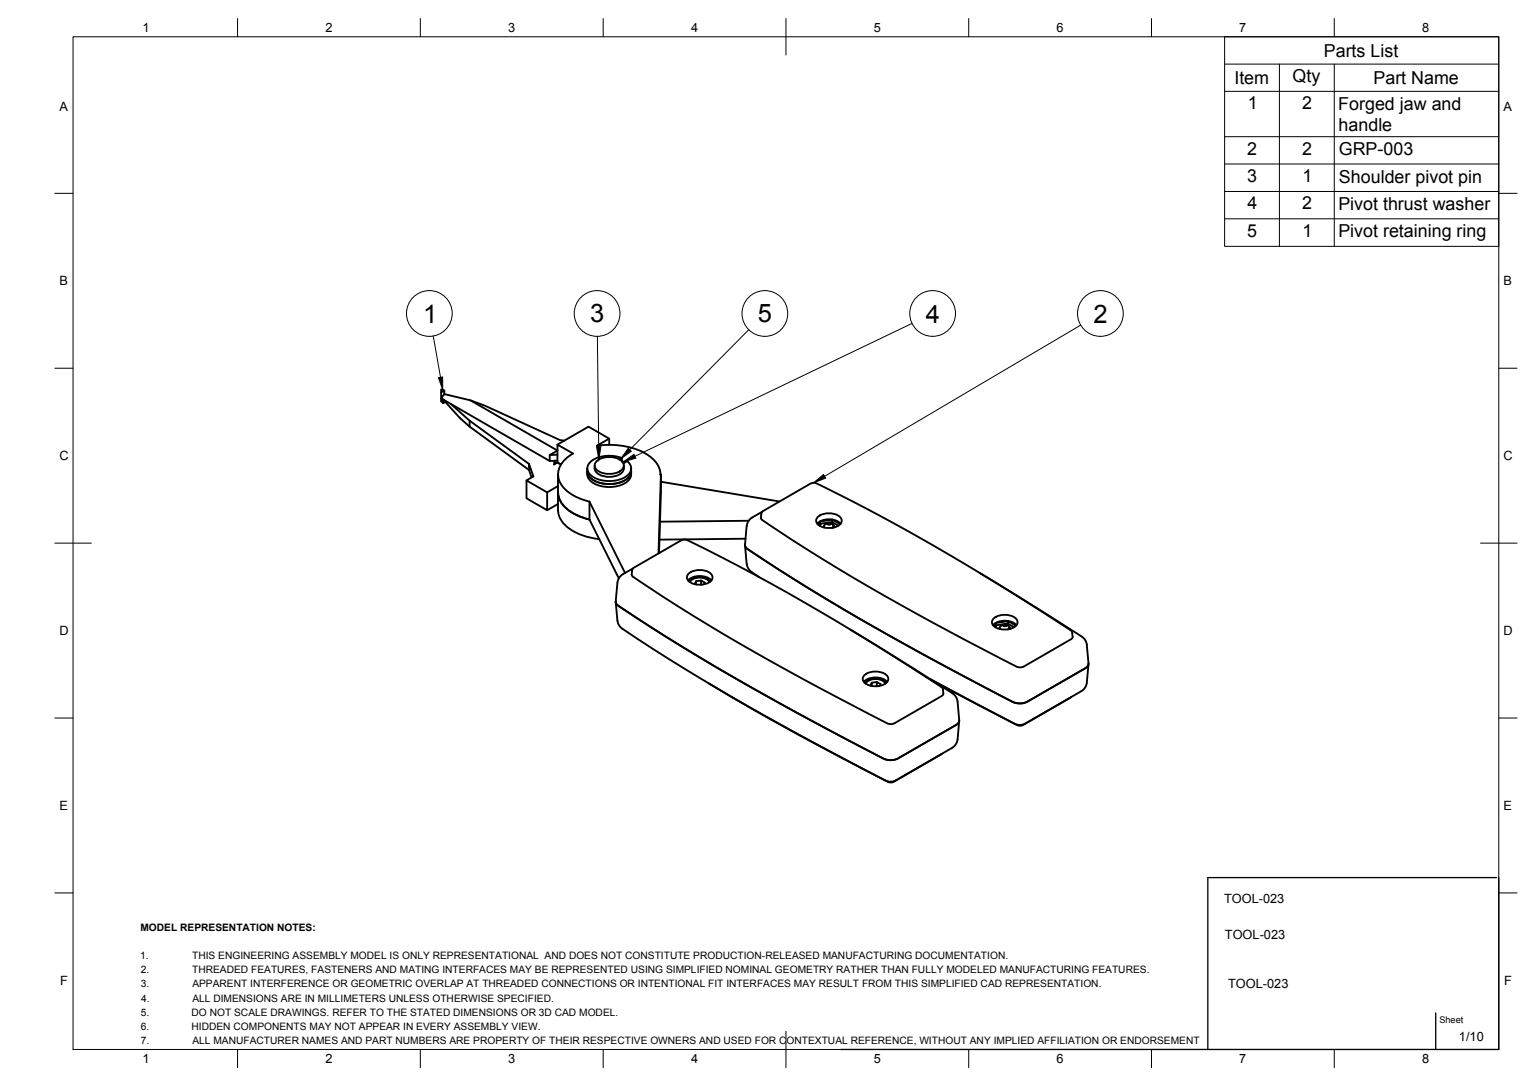
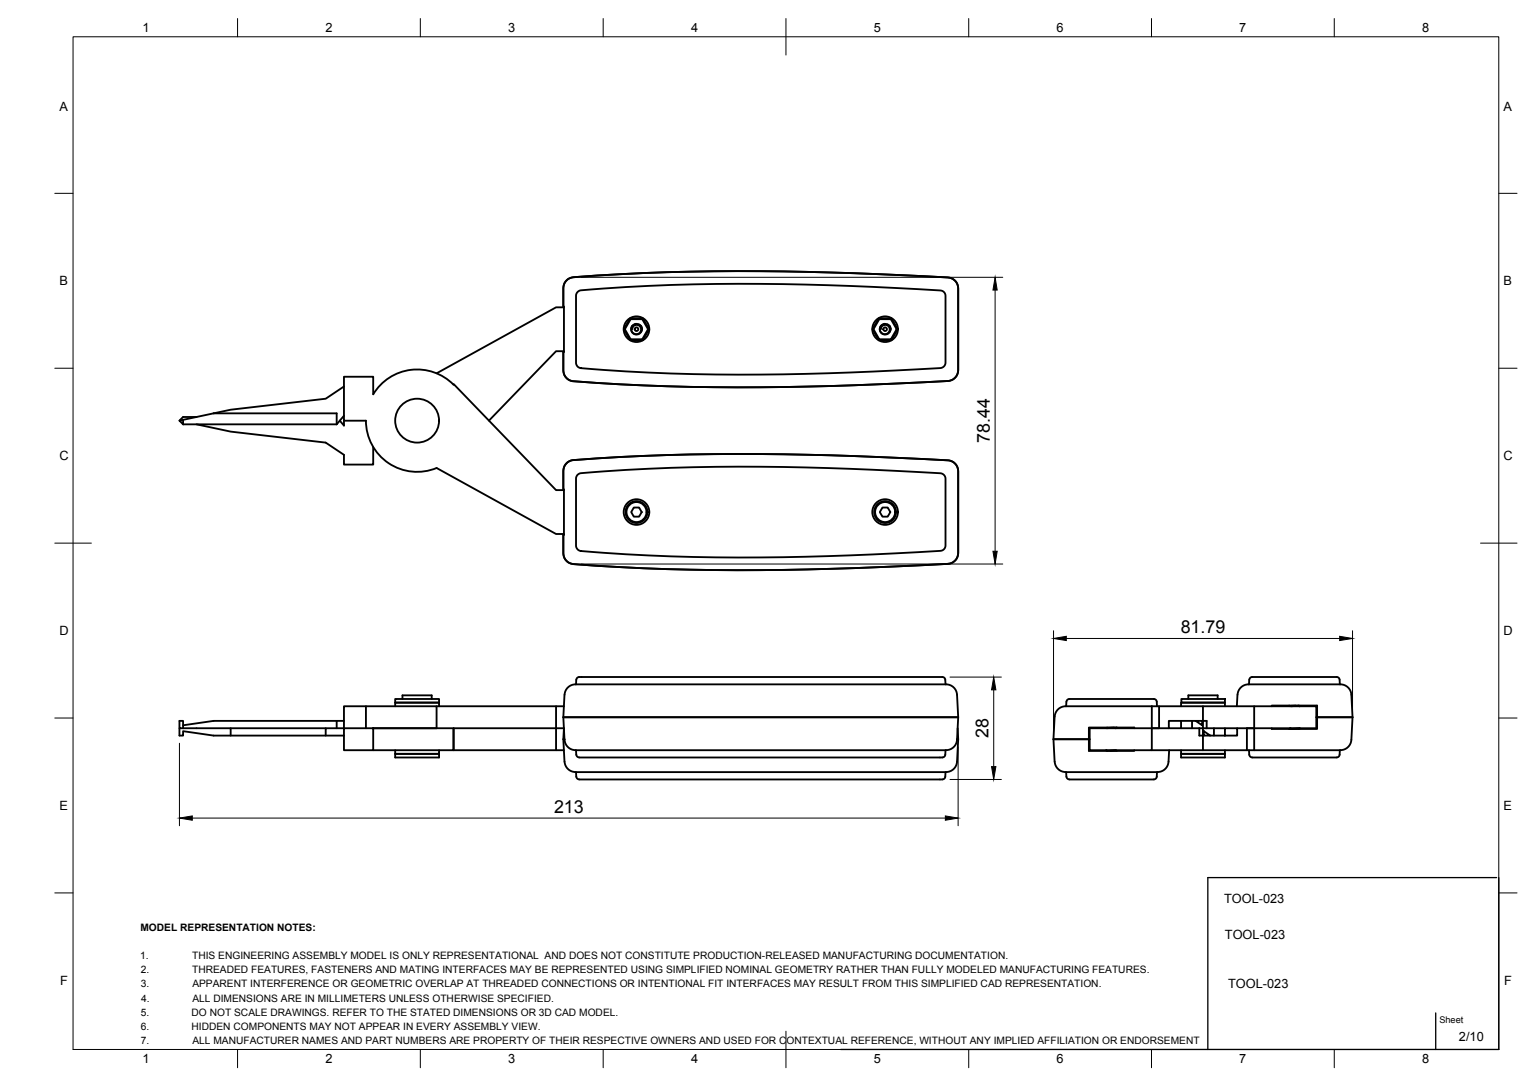
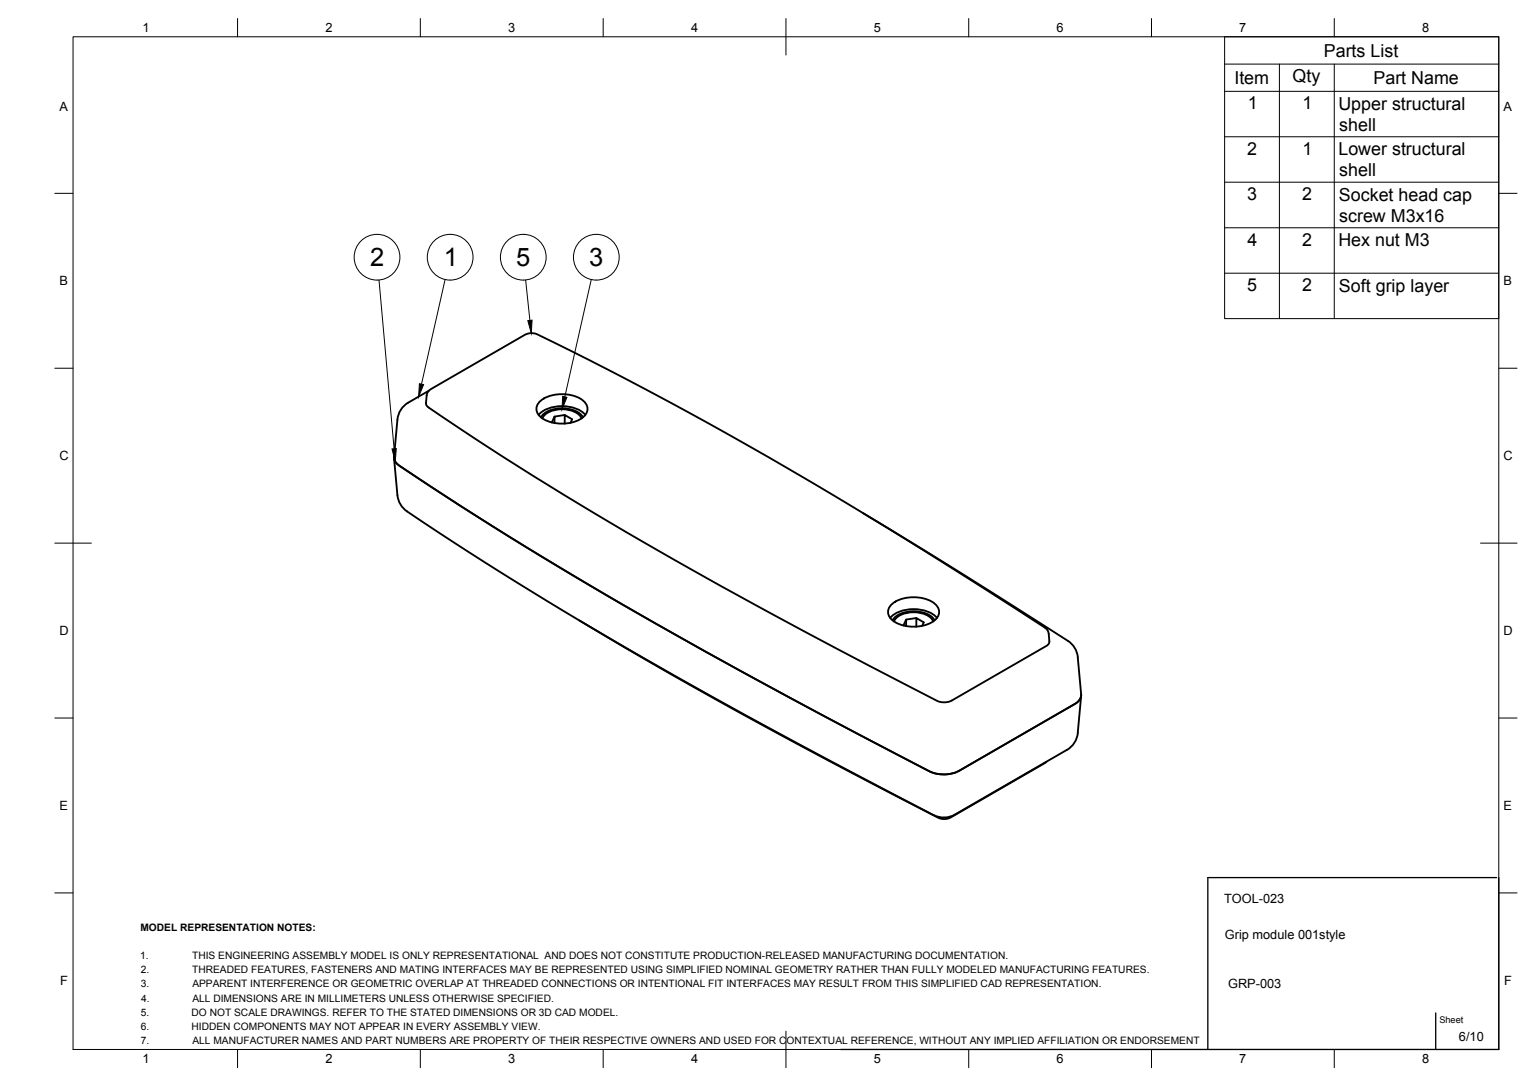
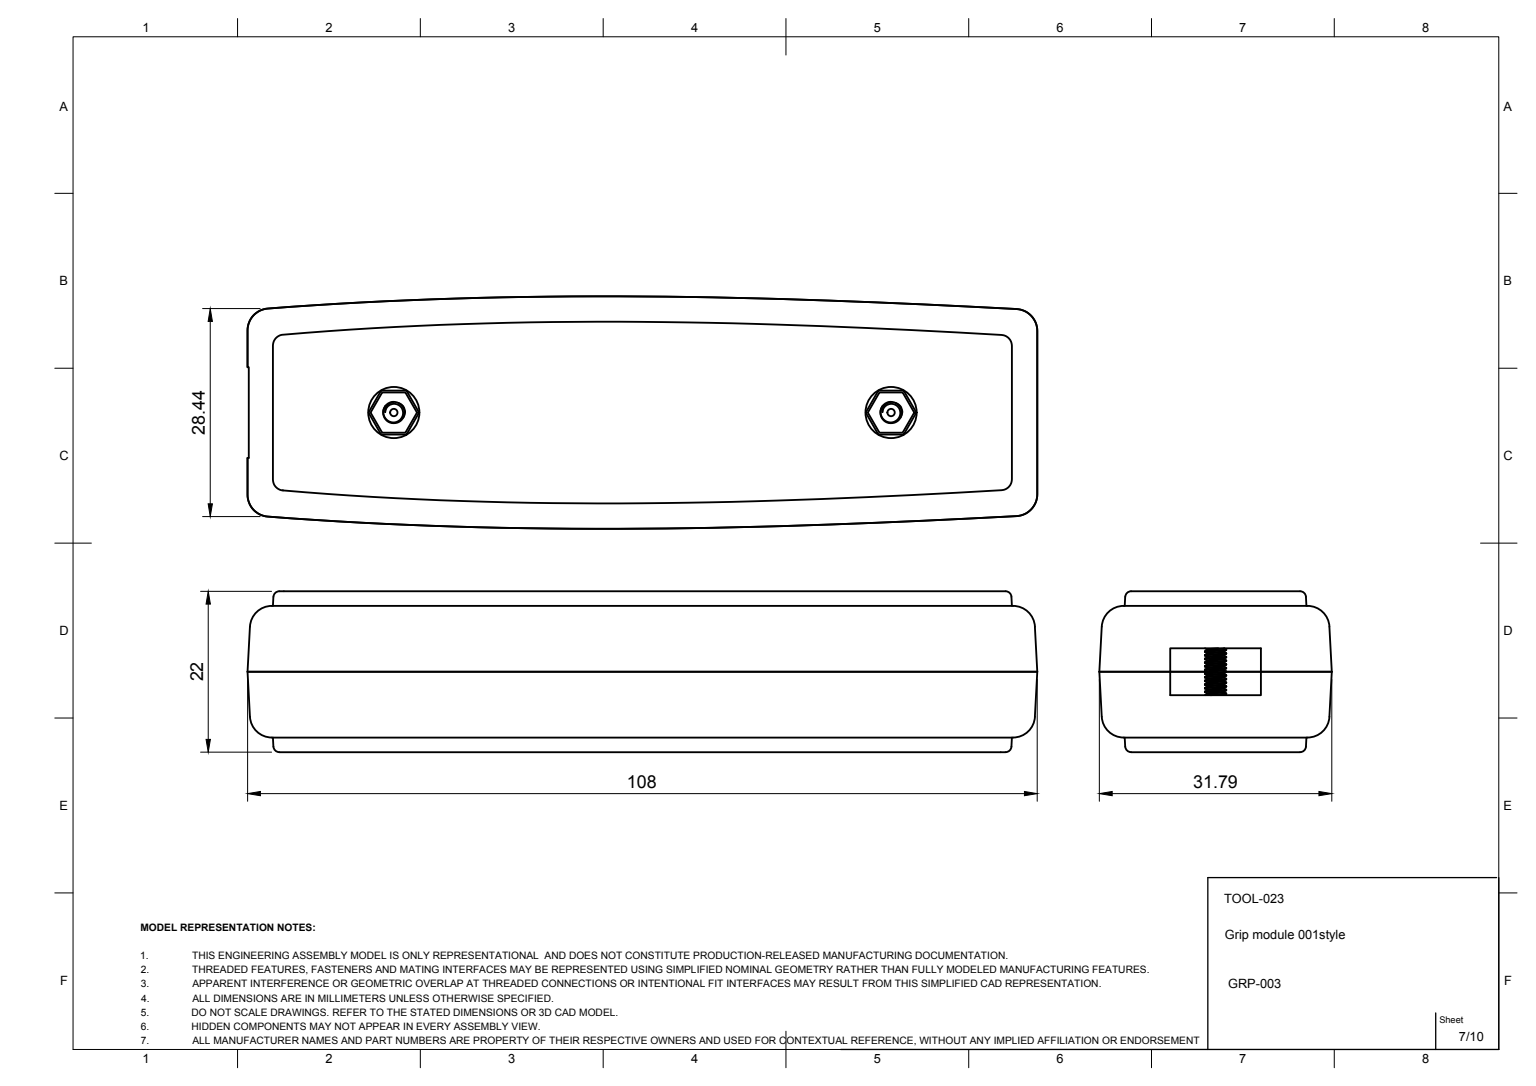
ISO-10303-21;
HEADER;
/* Generated by software containing ST-Developer
 * from STEP Tools, Inc. (www.steptools.com) 
 */

FILE_DESCRIPTION(
/* description */ (''),
/* implementation_level */ '2;1');

FILE_NAME(
/* name */ 'TOOL-023.step',
/* time_stamp */ '2026-11-10T05:40:20-08:00',
/* author */ (''),
/* organization */ (''),
/* preprocessor_version */ 'ST-DEVELOPER v20.2',
/* originating_system */ 'Autodesk Translation Framework v15.17.0.0',
/* authorisation */ '');

FILE_SCHEMA (('AUTOMOTIVE_DESIGN { 1 0 10303 214 3 1 1 }'));
ENDSEC;

DATA;
#10=MECHANICAL_DESIGN_GEOMETRIC_PRESENTATION_REPRESENTATION('',(#572,#573,
#574,#575,#576,#577,#578,#579,#580),#18580);
#11=ITEM_DEFINED_TRANSFORMATION($,$,#6722,#7109);
#12=ITEM_DEFINED_TRANSFORMATION($,$,#6832,#7110);
#13=ITEM_DEFINED_TRANSFORMATION($,$,#6948,#7111);
#14=ITEM_DEFINED_TRANSFORMATION($,$,#7030,#7112);
#15=ITEM_DEFINED_TRANSFORMATION($,$,#7056,#7113);
#16=ITEM_DEFINED_TRANSFORMATION($,$,#6948,#7114);
#17=ITEM_DEFINED_TRANSFORMATION($,$,#7030,#7115);
#18=ITEM_DEFINED_TRANSFORMATION($,$,#7056,#7116);
#19=ITEM_DEFINED_TRANSFORMATION($,$,#6654,#7126);
#20=ITEM_DEFINED_TRANSFORMATION($,$,#6721,#7127);
#21=ITEM_DEFINED_TRANSFORMATION($,$,#6654,#7128);
#22=ITEM_DEFINED_TRANSFORMATION($,$,#6692,#7129);
#23=ITEM_DEFINED_TRANSFORMATION($,$,#7117,#7130);
#24=ITEM_DEFINED_TRANSFORMATION($,$,#6710,#7131);
#25=ITEM_DEFINED_TRANSFORMATION($,$,#6721,#7132);
#26=ITEM_DEFINED_TRANSFORMATION($,$,#7117,#7133);
#27=(
REPRESENTATION_RELATIONSHIP($,$,#18628,#18627)
REPRESENTATION_RELATIONSHIP_WITH_TRANSFORMATION(#11)
SHAPE_REPRESENTATION_RELATIONSHIP()
);
#28=(
REPRESENTATION_RELATIONSHIP($,$,#18629,#18627)
REPRESENTATION_RELATIONSHIP_WITH_TRANSFORMATION(#12)
SHAPE_REPRESENTATION_RELATIONSHIP()
);
#29=(
REPRESENTATION_RELATIONSHIP($,$,#18630,#18627)
REPRESENTATION_RELATIONSHIP_WITH_TRANSFORMATION(#13)
SHAPE_REPRESENTATION_RELATIONSHIP()
);
#30=(
REPRESENTATION_RELATIONSHIP($,$,#18631,#18627)
REPRESENTATION_RELATIONSHIP_WITH_TRANSFORMATION(#14)
SHAPE_REPRESENTATION_RELATIONSHIP()
);
#31=(
REPRESENTATION_RELATIONSHIP($,$,#18632,#18627)
REPRESENTATION_RELATIONSHIP_WITH_TRANSFORMATION(#15)
SHAPE_REPRESENTATION_RELATIONSHIP()
);
#32=(
REPRESENTATION_RELATIONSHIP($,$,#18630,#18627)
REPRESENTATION_RELATIONSHIP_WITH_TRANSFORMATION(#16)
SHAPE_REPRESENTATION_RELATIONSHIP()
);
#33=(
REPRESENTATION_RELATIONSHIP($,$,#18631,#18627)
REPRESENTATION_RELATIONSHIP_WITH_TRANSFORMATION(#17)
SHAPE_REPRESENTATION_RELATIONSHIP()
);
#34=(
REPRESENTATION_RELATIONSHIP($,$,#18632,#18627)
REPRESENTATION_RELATIONSHIP_WITH_TRANSFORMATION(#18)
SHAPE_REPRESENTATION_RELATIONSHIP()
);
#35=(
REPRESENTATION_RELATIONSHIP($,$,#18624,#18623)
REPRESENTATION_RELATIONSHIP_WITH_TRANSFORMATION(#19)
SHAPE_REPRESENTATION_RELATIONSHIP()
);
#36=(
REPRESENTATION_RELATIONSHIP($,$,#18627,#18623)
REPRESENTATION_RELATIONSHIP_WITH_TRANSFORMATION(#20)
SHAPE_REPRESENTATION_RELATIONSHIP()
);
#37=(
REPRESENTATION_RELATIONSHIP($,$,#18624,#18623)
REPRESENTATION_RELATIONSHIP_WITH_TRANSFORMATION(#21)
SHAPE_REPRESENTATION_RELATIONSHIP()
);
#38=(
REPRESENTATION_RELATIONSHIP($,$,#18625,#18623)
REPRESENTATION_RELATIONSHIP_WITH_TRANSFORMATION(#22)
SHAPE_REPRESENTATION_RELATIONSHIP()
);
#39=(
REPRESENTATION_RELATIONSHIP($,$,#18633,#18623)
REPRESENTATION_RELATIONSHIP_WITH_TRANSFORMATION(#23)
SHAPE_REPRESENTATION_RELATIONSHIP()
);
#40=(
REPRESENTATION_RELATIONSHIP($,$,#18626,#18623)
REPRESENTATION_RELATIONSHIP_WITH_TRANSFORMATION(#24)
SHAPE_REPRESENTATION_RELATIONSHIP()
);
#41=(
REPRESENTATION_RELATIONSHIP($,$,#18627,#18623)
REPRESENTATION_RELATIONSHIP_WITH_TRANSFORMATION(#25)
SHAPE_REPRESENTATION_RELATIONSHIP()
);
#42=(
REPRESENTATION_RELATIONSHIP($,$,#18633,#18623)
REPRESENTATION_RELATIONSHIP_WITH_TRANSFORMATION(#26)
SHAPE_REPRESENTATION_RELATIONSHIP()
);
#43=CONTEXT_DEPENDENT_SHAPE_REPRESENTATION(#27,#18606);
#44=CONTEXT_DEPENDENT_SHAPE_REPRESENTATION(#28,#18607);
#45=CONTEXT_DEPENDENT_SHAPE_REPRESENTATION(#29,#18608);
#46=CONTEXT_DEPENDENT_SHAPE_REPRESENTATION(#30,#18609);
#47=CONTEXT_DEPENDENT_SHAPE_REPRESENTATION(#31,#18610);
#48=CONTEXT_DEPENDENT_SHAPE_REPRESENTATION(#32,#18611);
#49=CONTEXT_DEPENDENT_SHAPE_REPRESENTATION(#33,#18612);
#50=CONTEXT_DEPENDENT_SHAPE_REPRESENTATION(#34,#18613);
#51=CONTEXT_DEPENDENT_SHAPE_REPRESENTATION(#35,#18615);
#52=CONTEXT_DEPENDENT_SHAPE_REPRESENTATION(#36,#18616);
#53=CONTEXT_DEPENDENT_SHAPE_REPRESENTATION(#37,#18617);
#54=CONTEXT_DEPENDENT_SHAPE_REPRESENTATION(#38,#18618);
#55=CONTEXT_DEPENDENT_SHAPE_REPRESENTATION(#39,#18619);
#56=CONTEXT_DEPENDENT_SHAPE_REPRESENTATION(#40,#18620);
#57=CONTEXT_DEPENDENT_SHAPE_REPRESENTATION(#41,#18621);
#58=CONTEXT_DEPENDENT_SHAPE_REPRESENTATION(#42,#18622);
#59=NEXT_ASSEMBLY_USAGE_OCCURRENCE('Upper structural shell:1',
'Upper structural shell:1','Upper structural shell:1',#18639,#18640,
'Upper structural shell:1');
#60=NEXT_ASSEMBLY_USAGE_OCCURRENCE('Lower structural shell:1',
'Lower structural shell:1','Lower structural shell:1',#18639,#18641,
'Lower structural shell:1');
#61=NEXT_ASSEMBLY_USAGE_OCCURRENCE('Socket head cap screw M3x16:1',
'Socket head cap screw M3x16:1','Socket head cap screw M3x16:1',#18639,
#18642,'Socket head cap screw M3x16:1');
#62=NEXT_ASSEMBLY_USAGE_OCCURRENCE('Hex nut M3:1','Hex nut M3:1',
'Hex nut M3:1',#18639,#18643,'Hex nut M3:1');
#63=NEXT_ASSEMBLY_USAGE_OCCURRENCE('Soft grip layer:1',
'Soft grip layer:1','Soft grip layer:1',#18639,#18644,
'Soft grip layer:1');
#64=NEXT_ASSEMBLY_USAGE_OCCURRENCE('Socket head cap screw M3x16:2',
'Socket head cap screw M3x16:2','Socket head cap screw M3x16:2',#18639,
#18642,'Socket head cap screw M3x16:2');
#65=NEXT_ASSEMBLY_USAGE_OCCURRENCE('Hex nut M3:2','Hex nut M3:2',
'Hex nut M3:2',#18639,#18643,'Hex nut M3:2');
#66=NEXT_ASSEMBLY_USAGE_OCCURRENCE('Soft grip layer:2',
'Soft grip layer:2','Soft grip layer:2',#18639,#18644,
'Soft grip layer:2');
#67=NEXT_ASSEMBLY_USAGE_OCCURRENCE('Forged jaw and handle:1',
'Forged jaw and handle:1','Forged jaw and handle:1',#18635,#18636,
'Forged jaw and handle:1');
#68=NEXT_ASSEMBLY_USAGE_OCCURRENCE('Grip module:1','Grip module:1',
'Grip module:1',#18635,#18639,'Grip module:1');
#69=NEXT_ASSEMBLY_USAGE_OCCURRENCE('Forged jaw and handle:2',
'Forged jaw and handle:2','Forged jaw and handle:2',#18635,#18636,
'Forged jaw and handle:2');
#70=NEXT_ASSEMBLY_USAGE_OCCURRENCE('Shoulder pivot pin:1',
'Shoulder pivot pin:1','Shoulder pivot pin:1',#18635,#18637,
'Shoulder pivot pin:1');
#71=NEXT_ASSEMBLY_USAGE_OCCURRENCE('Pivot thrust washer:1',
'Pivot thrust washer:1','Pivot thrust washer:1',#18635,#18645,
'Pivot thrust washer:1');
#72=NEXT_ASSEMBLY_USAGE_OCCURRENCE('Pivot retaining ring:1',
'Pivot retaining ring:1','Pivot retaining ring:1',#18635,#18638,
'Pivot retaining ring:1');
#73=NEXT_ASSEMBLY_USAGE_OCCURRENCE('Grip module:2','Grip module:2',
'Grip module:2',#18635,#18639,'Grip module:2');
#74=NEXT_ASSEMBLY_USAGE_OCCURRENCE('Pivot thrust washer:2',
'Pivot thrust washer:2','Pivot thrust washer:2',#18635,#18645,
'Pivot thrust washer:2');
#75=CONICAL_SURFACE('',#7011,0.1,0.785398163397448);
#76=SPHERICAL_SURFACE('',#6795,0.1);
#77=SPHERICAL_SURFACE('',#6798,0.0999999999999998);
#78=SPHERICAL_SURFACE('',#6802,0.0999999999999993);
#79=SPHERICAL_SURFACE('',#6806,0.1);
#80=SPHERICAL_SURFACE('',#6811,0.3);
#81=SPHERICAL_SURFACE('',#6815,0.3);
#82=SPHERICAL_SURFACE('',#6819,0.299999999999999);
#83=SPHERICAL_SURFACE('',#6824,0.3);
#84=SPHERICAL_SURFACE('',#6911,0.1);
#85=SPHERICAL_SURFACE('',#6914,0.0999999999999998);
#86=SPHERICAL_SURFACE('',#6918,0.0999999999999993);
#87=SPHERICAL_SURFACE('',#6922,0.1);
#88=SPHERICAL_SURFACE('',#6927,0.3);
#89=SPHERICAL_SURFACE('',#6931,0.3);
#90=SPHERICAL_SURFACE('',#6935,0.299999999999999);
#91=SPHERICAL_SURFACE('',#6940,0.3);
#92=B_SPLINE_SURFACE_WITH_KNOTS('',3,3,((#8816,#8817,#8818,#8819),(#8820,
#8821,#8822,#8823),(#8824,#8825,#8826,#8827),(#8828,#8829,#8830,#8831),
(#8832,#8833,#8834,#8835)),.UNSPECIFIED.,.F.,.F.,.F.,(4,1,4),(4,4),(0.,
0.571428571428571,1.),(1.0454440030657,3.44967454744645),.UNSPECIFIED.);
#93=B_SPLINE_SURFACE_WITH_KNOTS('',3,3,((#8908,#8909,#8910,#8911),(#8912,
#8913,#8914,#8915),(#8916,#8917,#8918,#8919),(#8920,#8921,#8922,#8923),
(#8924,#8925,#8926,#8927)),.UNSPECIFIED.,.F.,.F.,.F.,(4,1,4),(4,4),(0.,
0.571428571428571,1.),(7.24519303641511,9.95046872158573),.UNSPECIFIED.);
#94=B_SPLINE_SURFACE_WITH_KNOTS('',3,3,((#9789,#9790,#9791,#9792),(#9793,
#9794,#9795,#9796),(#9797,#9798,#9799,#9800),(#9801,#9802,#9803,#9804)),
 .UNSPECIFIED.,.F.,.F.,.F.,(4,4),(4,4),(0.0705535719740953,0.323522444336189),
(0.0117434863834119,0.684857763552191),.UNSPECIFIED.);
#95=B_SPLINE_SURFACE_WITH_KNOTS('',3,3,((#9809,#9810,#9811,#9812),(#9813,
#9814,#9815,#9816),(#9817,#9818,#9819,#9820),(#9821,#9822,#9823,#9824)),
 .UNSPECIFIED.,.F.,.F.,.F.,(4,4),(4,4),(0.0262419052680539,0.0545428296147404),
(0.0121538053864343,0.684980602226481),.UNSPECIFIED.);
#96=B_SPLINE_SURFACE_WITH_KNOTS('',3,3,((#9834,#9835,#9836,#9837),(#9838,
#9839,#9840,#9841),(#9842,#9843,#9844,#9845),(#9846,#9847,#9848,#9849),
(#9850,#9851,#9852,#9853)),.UNSPECIFIED.,.F.,.F.,.F.,(4,1,4),(4,4),(0.,
0.571428571428571,1.),(0.752061768057538,3.45733745322815),
 .UNSPECIFIED.);
#97=B_SPLINE_SURFACE_WITH_KNOTS('',3,3,((#9854,#9855,#9856,#9857),(#9858,
#9859,#9860,#9861),(#9862,#9863,#9864,#9865),(#9866,#9867,#9868,#9869),
(#9870,#9871,#9872,#9873)),.UNSPECIFIED.,.F.,.F.,.F.,(4,1,4),(4,4),(0.,
0.571428571428571,1.),(0.283259008618247,0.557056952888827),
 .UNSPECIFIED.);
#98=B_SPLINE_SURFACE_WITH_KNOTS('',3,3,((#9887,#9888,#9889,#9890),(#9891,
#9892,#9893,#9894),(#9895,#9896,#9897,#9898),(#9899,#9900,#9901,#9902)),
 .UNSPECIFIED.,.F.,.F.,.F.,(4,4),(4,4),(0.67647755566375,0.929446428026011),
(0.0117434863436937,0.684857763580381),.UNSPECIFIED.);
#99=B_SPLINE_SURFACE_WITH_KNOTS('',3,3,((#9903,#9904,#9905,#9906),(#9907,
#9908,#9909,#9910),(#9911,#9912,#9913,#9914),(#9915,#9916,#9917,#9918)),
 .UNSPECIFIED.,.F.,.F.,.F.,(4,4),(4,4),(0.945457170385156,0.973758094731946),
(0.0121538053598088,0.684980602226481),.UNSPECIFIED.);
#100=B_SPLINE_SURFACE_WITH_KNOTS('',3,3,((#10002,#10003,#10004,#10005),
(#10006,#10007,#10008,#10009),(#10010,#10011,#10012,#10013),(#10014,#10015,
#10016,#10017)),.UNSPECIFIED.,.F.,.F.,.F.,(4,4),(4,4),(0.341142793678372,
0.658675488550287),(0.0116221239297273,0.684255166525269),.UNSPECIFIED.);
#101=B_SPLINE_SURFACE_WITH_KNOTS('',3,3,((#10022,#10023,#10024,#10025),
(#10026,#10027,#10028,#10029),(#10030,#10031,#10032,#10033),(#10034,#10035,
#10036,#10037),(#10038,#10039,#10040,#10041)),.UNSPECIFIED.,.F.,.F.,.F.,
(4,1,4),(4,4),(0.,0.571428571428571,1.),(3.65450559744172,7.0548588409572),
 .UNSPECIFIED.);
#102=B_SPLINE_SURFACE_WITH_KNOTS('',3,3,((#10051,#10052,#10053,#10054),
(#10055,#10056,#10057,#10058),(#10059,#10060,#10061,#10062),(#10063,#10064,
#10065,#10066),(#10067,#10068,#10069,#10070)),.UNSPECIFIED.,.F.,.F.,.F.,
(4,1,4),(4,4),(0.,0.571428571428571,1.),(3.64767164868607,7.04802489220155),
 .UNSPECIFIED.);
#103=B_SPLINE_SURFACE_WITH_KNOTS('',3,3,((#10075,#10076,#10077,#10078),
(#10079,#10080,#10081,#10082),(#10083,#10084,#10085,#10086),(#10087,#10088,
#10089,#10090)),.UNSPECIFIED.,.F.,.F.,.F.,(4,4),(4,4),(0.341324511449716,
0.658857206321627),(0.0116221214776208,0.684255166525269),.UNSPECIFIED.);
#104=B_SPLINE_SURFACE_WITH_KNOTS('',3,3,((#10135,#10136,#10137,#10138),
(#10139,#10140,#10141,#10142),(#10143,#10144,#10145,#10146),(#10147,#10148,
#10149,#10150)),.UNSPECIFIED.,.F.,.F.,.F.,(4,4),(4,4),(0.676316266718331,
0.901708040522105),(0.0117102006467275,0.68495201331719),.UNSPECIFIED.);
#105=B_SPLINE_SURFACE_WITH_KNOTS('',3,3,((#10155,#10156,#10157,#10158),
(#10159,#10160,#10161,#10162),(#10163,#10164,#10165,#10166),(#10167,#10168,
#10169,#10170),(#10171,#10172,#10173,#10174)),.UNSPECIFIED.,.F.,.F.,.F.,
(4,1,4),(4,4),(0.,0.571428571428571,1.),(7.25285594219682,9.65708648657758),
 .UNSPECIFIED.);
#106=B_SPLINE_SURFACE_WITH_KNOTS('',3,3,((#10184,#10185,#10186,#10187),
(#10188,#10189,#10190,#10191),(#10192,#10193,#10194,#10195),(#10196,#10197,
#10198,#10199)),.UNSPECIFIED.,.F.,.F.,.F.,(4,4),(4,4),(0.0982919594778951,
0.323683733281714),(0.0117102006467272,0.68495201331719),.UNSPECIFIED.);
#107=B_SPLINE_SURFACE_WITH_KNOTS('',3,3,((#10274,#10275,#10276,#10277),
(#10278,#10279,#10280,#10281),(#10282,#10283,#10284,#10285),(#10286,#10287,
#10288,#10289)),.UNSPECIFIED.,.F.,.F.,.F.,(4,4),(4,4),(0.917922863855343,
0.974411608827007),(0.0122403473423911,0.685344304754238),.UNSPECIFIED.);
#108=B_SPLINE_SURFACE_WITH_KNOTS('',3,3,((#10299,#10300,#10301,#10302),
(#10303,#10304,#10305,#10306),(#10307,#10308,#10309,#10310),(#10311,#10312,
#10313,#10314),(#10315,#10316,#10317,#10318)),.UNSPECIFIED.,.F.,.F.,.F.,
(4,1,4),(4,4),(0.,0.571428571428571,1.),(9.85085636625011,10.4271318523291),
 .UNSPECIFIED.);
#109=B_SPLINE_SURFACE_WITH_KNOTS('',3,3,((#10332,#10333,#10334,#10335),
(#10336,#10337,#10338,#10339),(#10340,#10341,#10342,#10343),(#10344,#10345,
#10346,#10347)),.UNSPECIFIED.,.F.,.F.,.F.,(4,4),(4,4),(0.025588391172993,
0.0820771361446569),(0.0122403473423911,0.685344304754238),
 .UNSPECIFIED.);
#110=B_SPLINE_SURFACE_WITH_KNOTS('',3,3,((#10357,#10358,#10359,#10360),
(#10361,#10362,#10363,#10364),(#10365,#10366,#10367,#10368),(#10369,#10370,
#10371,#10372),(#10373,#10374,#10375,#10376)),.UNSPECIFIED.,.F.,.F.,.F.,
(4,1,4),(4,4),(0.,0.571428571428571,1.),(0.27539863731415,0.851674123393175),
 .UNSPECIFIED.);
#111=B_SPLINE_SURFACE_WITH_KNOTS('',3,3,((#10390,#10391,#10392,#10393),
(#10394,#10395,#10396,#10397),(#10398,#10399,#10400,#10401),(#10402,#10403,
#10404,#10405),(#10406,#10407,#10408,#10409)),.UNSPECIFIED.,.F.,.F.,.F.,
(4,1,4),(4,4),(0.,0.571428571428571,1.),(0.00944995813270487,0.618489359031386),
 .UNSPECIFIED.);
#112=B_SPLINE_SURFACE_WITH_KNOTS('',3,3,((#10416,#10417,#10418,#10419),
(#10420,#10421,#10422,#10423),(#10424,#10425,#10426,#10427),(#10428,#10429,
#10430,#10431),(#10432,#10433,#10434,#10435)),.UNSPECIFIED.,.F.,.F.,.F.,
(4,1,4),(4,4),(0.,0.571428571428571,1.),(0.00908570715245136,0.618164468641375),
 .UNSPECIFIED.);
#113=B_SPLINE_SURFACE_WITH_KNOTS('',3,3,((#10440,#10441,#10442,#10443),
(#10444,#10445,#10446,#10447),(#10448,#10449,#10450,#10451),(#10452,#10453,
#10454,#10455),(#10456,#10457,#10458,#10459)),.UNSPECIFIED.,.F.,.F.,.F.,
(4,1,4),(4,4),(0.,0.571428571428571,1.),(0.0091183540525243,0.618164468641375),
 .UNSPECIFIED.);
#114=B_SPLINE_SURFACE_WITH_KNOTS('',3,3,((#10464,#10465,#10466,#10467),
(#10468,#10469,#10470,#10471),(#10472,#10473,#10474,#10475),(#10476,#10477,
#10478,#10479),(#10480,#10481,#10482,#10483)),.UNSPECIFIED.,.F.,.F.,.F.,
(4,1,4),(4,4),(0.,0.571428571428571,1.),(10.1454735367545,10.419271481025),
 .UNSPECIFIED.);
#115=B_SPLINE_SURFACE_WITH_KNOTS('',3,3,((#10484,#10485,#10486,#10487),
(#10488,#10489,#10490,#10491),(#10492,#10493,#10494,#10495),(#10496,#10497,
#10498,#10499),(#10500,#10501,#10502,#10503)),.UNSPECIFIED.,.F.,.F.,.F.,
(4,1,4),(4,4),(0.,0.571428571428571,1.),(0.0094045468285345,0.618489359031386),
 .UNSPECIFIED.);
#116=B_SPLINE_SURFACE_WITH_KNOTS('',3,3,((#10529,#10530,#10531,#10532),
(#10533,#10534,#10535,#10536),(#10537,#10538,#10539,#10540),(#10541,#10542,
#10543,#10544),(#10545,#10546,#10547,#10548)),.UNSPECIFIED.,.F.,.F.,.F.,
(4,1,4),(4,4),(0.,0.571428571428571,1.),(-0.00535061636073277,0.618489359031386),
 .UNSPECIFIED.);
#117=B_SPLINE_SURFACE_WITH_KNOTS('',3,3,((#10567,#10568,#10569,#10570,#10571),
(#10572,#10573,#10574,#10575,#10576),(#10577,#10578,#10579,#10580,#10581),
(#10582,#10583,#10584,#10585,#10586),(#10587,#10588,#10589,#10590,#10591)),
 .UNSPECIFIED.,.F.,.F.,.F.,(4,1,4),(4,1,4),(0.,0.571428571428571,1.),(0.283259008618247,
4.63063308449434,10.4271318523291),.UNSPECIFIED.);
#118=B_SPLINE_SURFACE_WITH_KNOTS('',3,3,((#10602,#10603,#10604,#10605),
(#10606,#10607,#10608,#10609),(#10610,#10611,#10612,#10613),(#10614,#10615,
#10616,#10617),(#10618,#10619,#10620,#10621)),.UNSPECIFIED.,.F.,.F.,.F.,
(4,1,4),(4,4),(0.,0.571428571428571,1.),(-0.00578978989683084,0.618164468641375),
 .UNSPECIFIED.);
#119=B_SPLINE_SURFACE_WITH_KNOTS('',3,3,((#10630,#10631,#10632,#10633),
(#10634,#10635,#10636,#10637),(#10638,#10639,#10640,#10641),(#10642,#10643,
#10644,#10645),(#10646,#10647,#10648,#10649)),.UNSPECIFIED.,.F.,.F.,.F.,
(4,1,4),(4,4),(0.,0.571428571428571,1.),(-0.00569189159989896,0.618164468641375),
 .UNSPECIFIED.);
#120=B_SPLINE_SURFACE_WITH_KNOTS('',3,3,((#10658,#10659,#10660,#10661,#10662),
(#10663,#10664,#10665,#10666,#10667),(#10668,#10669,#10670,#10671,#10672),
(#10673,#10674,#10675,#10676,#10677),(#10678,#10679,#10680,#10681,#10682)),
 .UNSPECIFIED.,.F.,.F.,.F.,(4,1,4),(4,1,4),(0.,0.571428571428571,1.),(0.27539863731415,
4.62277271319024,10.419271481025),.UNSPECIFIED.);
#121=B_SPLINE_SURFACE_WITH_KNOTS('',3,3,((#10693,#10694,#10695,#10696),
(#10697,#10698,#10699,#10700),(#10701,#10702,#10703,#10704),(#10705,#10706,
#10707,#10708),(#10709,#10710,#10711,#10712)),.UNSPECIFIED.,.F.,.F.,.F.,
(4,1,4),(4,4),(0.,0.571428571428571,1.),(-0.0054868135546625,0.618489359031386),
 .UNSPECIFIED.);
#122=B_SPLINE_SURFACE_WITH_KNOTS('',3,3,((#10721,#10722,#10723,#10724),
(#10725,#10726,#10727,#10728),(#10729,#10730,#10731,#10732),(#10733,#10734,
#10735,#10736)),.UNSPECIFIED.,.F.,.F.,.F.,(4,4),(4,4),(0.026239262514127,
0.974414173651419),(0.,0.685344304754238),.UNSPECIFIED.);
#123=B_SPLINE_SURFACE_WITH_KNOTS('',3,3,((#10739,#10740,#10741,#10742),
(#10743,#10744,#10745,#10746),(#10747,#10748,#10749,#10750),(#10751,#10752,
#10753,#10754)),.UNSPECIFIED.,.F.,.F.,.F.,(4,4),(4,4),(0.0255858263485814,
0.973760737485873),(0.,0.685344304754238),.UNSPECIFIED.);
#124=B_SPLINE_SURFACE_WITH_KNOTS('',3,3,((#10861,#10862,#10863,#10864),
(#10865,#10866,#10867,#10868),(#10869,#10870,#10871,#10872),(#10873,#10874,
#10875,#10876),(#10877,#10878,#10879,#10880)),.UNSPECIFIED.,.F.,.F.,.F.,
(4,1,4),(4,4),(0.,0.571428571428571,1.),(1.0454440030657,3.44967454744645),
 .UNSPECIFIED.);
#125=B_SPLINE_SURFACE_WITH_KNOTS('',3,3,((#10953,#10954,#10955,#10956),
(#10957,#10958,#10959,#10960),(#10961,#10962,#10963,#10964),(#10965,#10966,
#10967,#10968),(#10969,#10970,#10971,#10972)),.UNSPECIFIED.,.F.,.F.,.F.,
(4,1,4),(4,4),(0.,0.571428571428571,1.),(7.24519303641511,9.95046872158573),
 .UNSPECIFIED.);
#126=B_SPLINE_SURFACE_WITH_KNOTS('',3,3,((#11894,#11895,#11896,#11897),
(#11898,#11899,#11900,#11901),(#11902,#11903,#11904,#11905),(#11906,#11907,
#11908,#11909)),.UNSPECIFIED.,.F.,.F.,.F.,(4,4),(4,4),(0.0705535719740953,
0.323522444336189),(0.0117434863834119,0.684857763552191),.UNSPECIFIED.);
#127=B_SPLINE_SURFACE_WITH_KNOTS('',3,3,((#11914,#11915,#11916,#11917),
(#11918,#11919,#11920,#11921),(#11922,#11923,#11924,#11925),(#11926,#11927,
#11928,#11929)),.UNSPECIFIED.,.F.,.F.,.F.,(4,4),(4,4),(0.0262419052680539,
0.0545428296147404),(0.0121538053864343,0.684980602226481),
 .UNSPECIFIED.);
#128=B_SPLINE_SURFACE_WITH_KNOTS('',3,3,((#11939,#11940,#11941,#11942),
(#11943,#11944,#11945,#11946),(#11947,#11948,#11949,#11950),(#11951,#11952,
#11953,#11954),(#11955,#11956,#11957,#11958)),.UNSPECIFIED.,.F.,.F.,.F.,
(4,1,4),(4,4),(0.,0.571428571428571,1.),(0.752061768057538,3.45733745322815),
 .UNSPECIFIED.);
#129=B_SPLINE_SURFACE_WITH_KNOTS('',3,3,((#11959,#11960,#11961,#11962),
(#11963,#11964,#11965,#11966),(#11967,#11968,#11969,#11970),(#11971,#11972,
#11973,#11974),(#11975,#11976,#11977,#11978)),.UNSPECIFIED.,.F.,.F.,.F.,
(4,1,4),(4,4),(0.,0.571428571428571,1.),(0.283259008618247,0.557056952888827),
 .UNSPECIFIED.);
#130=B_SPLINE_SURFACE_WITH_KNOTS('',3,3,((#11992,#11993,#11994,#11995),
(#11996,#11997,#11998,#11999),(#12000,#12001,#12002,#12003),(#12004,#12005,
#12006,#12007)),.UNSPECIFIED.,.F.,.F.,.F.,(4,4),(4,4),(0.67647755566375,
0.929446428026011),(0.0117434863436937,0.684857763580381),.UNSPECIFIED.);
#131=B_SPLINE_SURFACE_WITH_KNOTS('',3,3,((#12008,#12009,#12010,#12011),
(#12012,#12013,#12014,#12015),(#12016,#12017,#12018,#12019),(#12020,#12021,
#12022,#12023)),.UNSPECIFIED.,.F.,.F.,.F.,(4,4),(4,4),(0.945457170385156,
0.973758094731946),(0.0121538053598088,0.684980602226481),.UNSPECIFIED.);
#132=B_SPLINE_SURFACE_WITH_KNOTS('',3,3,((#12107,#12108,#12109,#12110),
(#12111,#12112,#12113,#12114),(#12115,#12116,#12117,#12118),(#12119,#12120,
#12121,#12122)),.UNSPECIFIED.,.F.,.F.,.F.,(4,4),(4,4),(0.341142793678372,
0.658675488550287),(0.0116221239297273,0.684255166525269),.UNSPECIFIED.);
#133=B_SPLINE_SURFACE_WITH_KNOTS('',3,3,((#12127,#12128,#12129,#12130),
(#12131,#12132,#12133,#12134),(#12135,#12136,#12137,#12138),(#12139,#12140,
#12141,#12142),(#12143,#12144,#12145,#12146)),.UNSPECIFIED.,.F.,.F.,.F.,
(4,1,4),(4,4),(0.,0.571428571428571,1.),(3.65450559744172,7.0548588409572),
 .UNSPECIFIED.);
#134=B_SPLINE_SURFACE_WITH_KNOTS('',3,3,((#12156,#12157,#12158,#12159),
(#12160,#12161,#12162,#12163),(#12164,#12165,#12166,#12167),(#12168,#12169,
#12170,#12171),(#12172,#12173,#12174,#12175)),.UNSPECIFIED.,.F.,.F.,.F.,
(4,1,4),(4,4),(0.,0.571428571428571,1.),(3.64767164868607,7.04802489220155),
 .UNSPECIFIED.);
#135=B_SPLINE_SURFACE_WITH_KNOTS('',3,3,((#12180,#12181,#12182,#12183),
(#12184,#12185,#12186,#12187),(#12188,#12189,#12190,#12191),(#12192,#12193,
#12194,#12195)),.UNSPECIFIED.,.F.,.F.,.F.,(4,4),(4,4),(0.341324511449716,
0.658857206321627),(0.0116221214776208,0.684255166525269),.UNSPECIFIED.);
#136=B_SPLINE_SURFACE_WITH_KNOTS('',3,3,((#12240,#12241,#12242,#12243),
(#12244,#12245,#12246,#12247),(#12248,#12249,#12250,#12251),(#12252,#12253,
#12254,#12255)),.UNSPECIFIED.,.F.,.F.,.F.,(4,4),(4,4),(0.676316266718331,
0.901708040522105),(0.0117102006467275,0.68495201331719),.UNSPECIFIED.);
#137=B_SPLINE_SURFACE_WITH_KNOTS('',3,3,((#12260,#12261,#12262,#12263),
(#12264,#12265,#12266,#12267),(#12268,#12269,#12270,#12271),(#12272,#12273,
#12274,#12275),(#12276,#12277,#12278,#12279)),.UNSPECIFIED.,.F.,.F.,.F.,
(4,1,4),(4,4),(0.,0.571428571428571,1.),(7.25285594219682,9.65708648657758),
 .UNSPECIFIED.);
#138=B_SPLINE_SURFACE_WITH_KNOTS('',3,3,((#12289,#12290,#12291,#12292),
(#12293,#12294,#12295,#12296),(#12297,#12298,#12299,#12300),(#12301,#12302,
#12303,#12304)),.UNSPECIFIED.,.F.,.F.,.F.,(4,4),(4,4),(0.0982919594778951,
0.323683733281714),(0.0117102006467272,0.68495201331719),.UNSPECIFIED.);
#139=B_SPLINE_SURFACE_WITH_KNOTS('',3,3,((#12379,#12380,#12381,#12382),
(#12383,#12384,#12385,#12386),(#12387,#12388,#12389,#12390),(#12391,#12392,
#12393,#12394)),.UNSPECIFIED.,.F.,.F.,.F.,(4,4),(4,4),(0.917922863855343,
0.974411608827007),(0.0122403473423911,0.685344304754238),.UNSPECIFIED.);
#140=B_SPLINE_SURFACE_WITH_KNOTS('',3,3,((#12404,#12405,#12406,#12407),
(#12408,#12409,#12410,#12411),(#12412,#12413,#12414,#12415),(#12416,#12417,
#12418,#12419),(#12420,#12421,#12422,#12423)),.UNSPECIFIED.,.F.,.F.,.F.,
(4,1,4),(4,4),(0.,0.571428571428571,1.),(9.85085636625011,10.4271318523291),
 .UNSPECIFIED.);
#141=B_SPLINE_SURFACE_WITH_KNOTS('',3,3,((#12437,#12438,#12439,#12440),
(#12441,#12442,#12443,#12444),(#12445,#12446,#12447,#12448),(#12449,#12450,
#12451,#12452)),.UNSPECIFIED.,.F.,.F.,.F.,(4,4),(4,4),(0.025588391172993,
0.0820771361446569),(0.0122403473423911,0.685344304754238),
 .UNSPECIFIED.);
#142=B_SPLINE_SURFACE_WITH_KNOTS('',3,3,((#12462,#12463,#12464,#12465),
(#12466,#12467,#12468,#12469),(#12470,#12471,#12472,#12473),(#12474,#12475,
#12476,#12477),(#12478,#12479,#12480,#12481)),.UNSPECIFIED.,.F.,.F.,.F.,
(4,1,4),(4,4),(0.,0.571428571428571,1.),(0.27539863731415,0.851674123393175),
 .UNSPECIFIED.);
#143=B_SPLINE_SURFACE_WITH_KNOTS('',3,3,((#12495,#12496,#12497,#12498),
(#12499,#12500,#12501,#12502),(#12503,#12504,#12505,#12506),(#12507,#12508,
#12509,#12510),(#12511,#12512,#12513,#12514)),.UNSPECIFIED.,.F.,.F.,.F.,
(4,1,4),(4,4),(0.,0.571428571428571,1.),(0.00944995813270487,0.618489359031386),
 .UNSPECIFIED.);
#144=B_SPLINE_SURFACE_WITH_KNOTS('',3,3,((#12521,#12522,#12523,#12524),
(#12525,#12526,#12527,#12528),(#12529,#12530,#12531,#12532),(#12533,#12534,
#12535,#12536),(#12537,#12538,#12539,#12540)),.UNSPECIFIED.,.F.,.F.,.F.,
(4,1,4),(4,4),(0.,0.571428571428571,1.),(0.00908570715245136,0.618164468641375),
 .UNSPECIFIED.);
#145=B_SPLINE_SURFACE_WITH_KNOTS('',3,3,((#12545,#12546,#12547,#12548),
(#12549,#12550,#12551,#12552),(#12553,#12554,#12555,#12556),(#12557,#12558,
#12559,#12560),(#12561,#12562,#12563,#12564)),.UNSPECIFIED.,.F.,.F.,.F.,
(4,1,4),(4,4),(0.,0.571428571428571,1.),(0.0091183540525243,0.618164468641375),
 .UNSPECIFIED.);
#146=B_SPLINE_SURFACE_WITH_KNOTS('',3,3,((#12569,#12570,#12571,#12572),
(#12573,#12574,#12575,#12576),(#12577,#12578,#12579,#12580),(#12581,#12582,
#12583,#12584),(#12585,#12586,#12587,#12588)),.UNSPECIFIED.,.F.,.F.,.F.,
(4,1,4),(4,4),(0.,0.571428571428571,1.),(10.1454735367545,10.419271481025),
 .UNSPECIFIED.);
#147=B_SPLINE_SURFACE_WITH_KNOTS('',3,3,((#12589,#12590,#12591,#12592),
(#12593,#12594,#12595,#12596),(#12597,#12598,#12599,#12600),(#12601,#12602,
#12603,#12604),(#12605,#12606,#12607,#12608)),.UNSPECIFIED.,.F.,.F.,.F.,
(4,1,4),(4,4),(0.,0.571428571428571,1.),(0.0094045468285345,0.618489359031386),
 .UNSPECIFIED.);
#148=B_SPLINE_SURFACE_WITH_KNOTS('',3,3,((#12634,#12635,#12636,#12637),
(#12638,#12639,#12640,#12641),(#12642,#12643,#12644,#12645),(#12646,#12647,
#12648,#12649),(#12650,#12651,#12652,#12653)),.UNSPECIFIED.,.F.,.F.,.F.,
(4,1,4),(4,4),(0.,0.571428571428571,1.),(-0.00535061636073277,0.618489359031386),
 .UNSPECIFIED.);
#149=B_SPLINE_SURFACE_WITH_KNOTS('',3,3,((#12672,#12673,#12674,#12675,#12676),
(#12677,#12678,#12679,#12680,#12681),(#12682,#12683,#12684,#12685,#12686),
(#12687,#12688,#12689,#12690,#12691),(#12692,#12693,#12694,#12695,#12696)),
 .UNSPECIFIED.,.F.,.F.,.F.,(4,1,4),(4,1,4),(0.,0.571428571428571,1.),(0.283259008618247,
4.63063308449434,10.4271318523291),.UNSPECIFIED.);
#150=B_SPLINE_SURFACE_WITH_KNOTS('',3,3,((#12707,#12708,#12709,#12710),
(#12711,#12712,#12713,#12714),(#12715,#12716,#12717,#12718),(#12719,#12720,
#12721,#12722),(#12723,#12724,#12725,#12726)),.UNSPECIFIED.,.F.,.F.,.F.,
(4,1,4),(4,4),(0.,0.571428571428571,1.),(-0.00578978989683084,0.618164468641375),
 .UNSPECIFIED.);
#151=B_SPLINE_SURFACE_WITH_KNOTS('',3,3,((#12735,#12736,#12737,#12738),
(#12739,#12740,#12741,#12742),(#12743,#12744,#12745,#12746),(#12747,#12748,
#12749,#12750),(#12751,#12752,#12753,#12754)),.UNSPECIFIED.,.F.,.F.,.F.,
(4,1,4),(4,4),(0.,0.571428571428571,1.),(-0.00569189159989896,0.618164468641375),
 .UNSPECIFIED.);
#152=B_SPLINE_SURFACE_WITH_KNOTS('',3,3,((#12763,#12764,#12765,#12766,#12767),
(#12768,#12769,#12770,#12771,#12772),(#12773,#12774,#12775,#12776,#12777),
(#12778,#12779,#12780,#12781,#12782),(#12783,#12784,#12785,#12786,#12787)),
 .UNSPECIFIED.,.F.,.F.,.F.,(4,1,4),(4,1,4),(0.,0.571428571428571,1.),(0.27539863731415,
4.62277271319024,10.419271481025),.UNSPECIFIED.);
#153=B_SPLINE_SURFACE_WITH_KNOTS('',3,3,((#12798,#12799,#12800,#12801),
(#12802,#12803,#12804,#12805),(#12806,#12807,#12808,#12809),(#12810,#12811,
#12812,#12813),(#12814,#12815,#12816,#12817)),.UNSPECIFIED.,.F.,.F.,.F.,
(4,1,4),(4,4),(0.,0.571428571428571,1.),(-0.0054868135546625,0.618489359031386),
 .UNSPECIFIED.);
#154=B_SPLINE_SURFACE_WITH_KNOTS('',3,3,((#12826,#12827,#12828,#12829),
(#12830,#12831,#12832,#12833),(#12834,#12835,#12836,#12837),(#12838,#12839,
#12840,#12841)),.UNSPECIFIED.,.F.,.F.,.F.,(4,4),(4,4),(0.026239262514127,
0.974414173651419),(0.,0.685344304754238),.UNSPECIFIED.);
#155=B_SPLINE_SURFACE_WITH_KNOTS('',3,3,((#12844,#12845,#12846,#12847),
(#12848,#12849,#12850,#12851),(#12852,#12853,#12854,#12855),(#12856,#12857,
#12858,#12859)),.UNSPECIFIED.,.F.,.F.,.F.,(4,4),(4,4),(0.0255858263485814,
0.973760737485873),(0.,0.685344304754238),.UNSPECIFIED.);
#156=B_SPLINE_SURFACE_WITH_KNOTS('',3,3,((#15243,#15244,#15245,#15246,#15247,
#15248,#15249,#15250,#15251,#15252,#15253,#15254,#15255,#15256,#15257,#15258,
#15259,#15260,#15261,#15262,#15263,#15264,#15265,#15266,#15267,#15268,#15269,
#15270,#15271,#15272,#15273,#15274,#15275,#15276,#15277,#15278,#15279,#15280,
#15281,#15282,#15283,#15284,#15285,#15286,#15287,#15288,#15289,#15290,#15291,
#15292,#15293,#15294,#15295,#15296,#15297,#15298,#15299,#15300,#15301,#15302,
#15303,#15304,#15305,#15306,#15307,#15308,#15309,#15310,#15311,#15312,#15313,
#15314,#15315,#15316,#15317,#15318,#15319,#15320,#15321,#15322,#15323,#15324,
#15325,#15326,#15327,#15328,#15329,#15330,#15331,#15332,#15333,#15334,#15335,
#15336,#15337,#15338,#15339,#15340,#15341,#15342,#15343,#15344,#15345,#15346,
#15347,#15348,#15349,#15350,#15351,#15352,#15353,#15354,#15355,#15356,#15357,
#15358,#15359,#15360,#15361,#15362,#15363,#15364,#15365,#15366,#15367,#15368,
#15369,#15370,#15371,#15372,#15373,#15374,#15375,#15376,#15377,#15378,#15379,
#15380,#15381,#15382,#15383,#15384,#15385,#15386,#15387,#15388,#15389,#15390,
#15391,#15392,#15393,#15394,#15395,#15396,#15397,#15398,#15399,#15400,#15401,
#15402,#15403,#15404,#15405,#15406,#15407,#15408,#15409,#15410,#15411,#15412,
#15413,#15414,#15415,#15416,#15417,#15418,#15419,#15420,#15421,#15422,#15423,
#15424,#15425,#15426,#15427,#15428,#15429,#15430,#15431,#15432,#15433,#15434,
#15435,#15436,#15437,#15438),(#15439,#15440,#15441,#15442,#15443,#15444,
#15445,#15446,#15447,#15448,#15449,#15450,#15451,#15452,#15453,#15454,#15455,
#15456,#15457,#15458,#15459,#15460,#15461,#15462,#15463,#15464,#15465,#15466,
#15467,#15468,#15469,#15470,#15471,#15472,#15473,#15474,#15475,#15476,#15477,
#15478,#15479,#15480,#15481,#15482,#15483,#15484,#15485,#15486,#15487,#15488,
#15489,#15490,#15491,#15492,#15493,#15494,#15495,#15496,#15497,#15498,#15499,
#15500,#15501,#15502,#15503,#15504,#15505,#15506,#15507,#15508,#15509,#15510,
#15511,#15512,#15513,#15514,#15515,#15516,#15517,#15518,#15519,#15520,#15521,
#15522,#15523,#15524,#15525,#15526,#15527,#15528,#15529,#15530,#15531,#15532,
#15533,#15534,#15535,#15536,#15537,#15538,#15539,#15540,#15541,#15542,#15543,
#15544,#15545,#15546,#15547,#15548,#15549,#15550,#15551,#15552,#15553,#15554,
#15555,#15556,#15557,#15558,#15559,#15560,#15561,#15562,#15563,#15564,#15565,
#15566,#15567,#15568,#15569,#15570,#15571,#15572,#15573,#15574,#15575,#15576,
#15577,#15578,#15579,#15580,#15581,#15582,#15583,#15584,#15585,#15586,#15587,
#15588,#15589,#15590,#15591,#15592,#15593,#15594,#15595,#15596,#15597,#15598,
#15599,#15600,#15601,#15602,#15603,#15604,#15605,#15606,#15607,#15608,#15609,
#15610,#15611,#15612,#15613,#15614,#15615,#15616,#15617,#15618,#15619,#15620,
#15621,#15622,#15623,#15624,#15625,#15626,#15627,#15628,#15629,#15630,#15631,
#15632,#15633,#15634),(#15635,#15636,#15637,#15638,#15639,#15640,#15641,
#15642,#15643,#15644,#15645,#15646,#15647,#15648,#15649,#15650,#15651,#15652,
#15653,#15654,#15655,#15656,#15657,#15658,#15659,#15660,#15661,#15662,#15663,
#15664,#15665,#15666,#15667,#15668,#15669,#15670,#15671,#15672,#15673,#15674,
#15675,#15676,#15677,#15678,#15679,#15680,#15681,#15682,#15683,#15684,#15685,
#15686,#15687,#15688,#15689,#15690,#15691,#15692,#15693,#15694,#15695,#15696,
#15697,#15698,#15699,#15700,#15701,#15702,#15703,#15704,#15705,#15706,#15707,
#15708,#15709,#15710,#15711,#15712,#15713,#15714,#15715,#15716,#15717,#15718,
#15719,#15720,#15721,#15722,#15723,#15724,#15725,#15726,#15727,#15728,#15729,
#15730,#15731,#15732,#15733,#15734,#15735,#15736,#15737,#15738,#15739,#15740,
#15741,#15742,#15743,#15744,#15745,#15746,#15747,#15748,#15749,#15750,#15751,
#15752,#15753,#15754,#15755,#15756,#15757,#15758,#15759,#15760,#15761,#15762,
#15763,#15764,#15765,#15766,#15767,#15768,#15769,#15770,#15771,#15772,#15773,
#15774,#15775,#15776,#15777,#15778,#15779,#15780,#15781,#15782,#15783,#15784,
#15785,#15786,#15787,#15788,#15789,#15790,#15791,#15792,#15793,#15794,#15795,
#15796,#15797,#15798,#15799,#15800,#15801,#15802,#15803,#15804,#15805,#15806,
#15807,#15808,#15809,#15810,#15811,#15812,#15813,#15814,#15815,#15816,#15817,
#15818,#15819,#15820,#15821,#15822,#15823,#15824,#15825,#15826,#15827,#15828,
#15829,#15830),(#15831,#15832,#15833,#15834,#15835,#15836,#15837,#15838,
#15839,#15840,#15841,#15842,#15843,#15844,#15845,#15846,#15847,#15848,#15849,
#15850,#15851,#15852,#15853,#15854,#15855,#15856,#15857,#15858,#15859,#15860,
#15861,#15862,#15863,#15864,#15865,#15866,#15867,#15868,#15869,#15870,#15871,
#15872,#15873,#15874,#15875,#15876,#15877,#15878,#15879,#15880,#15881,#15882,
#15883,#15884,#15885,#15886,#15887,#15888,#15889,#15890,#15891,#15892,#15893,
#15894,#15895,#15896,#15897,#15898,#15899,#15900,#15901,#15902,#15903,#15904,
#15905,#15906,#15907,#15908,#15909,#15910,#15911,#15912,#15913,#15914,#15915,
#15916,#15917,#15918,#15919,#15920,#15921,#15922,#15923,#15924,#15925,#15926,
#15927,#15928,#15929,#15930,#15931,#15932,#15933,#15934,#15935,#15936,#15937,
#15938,#15939,#15940,#15941,#15942,#15943,#15944,#15945,#15946,#15947,#15948,
#15949,#15950,#15951,#15952,#15953,#15954,#15955,#15956,#15957,#15958,#15959,
#15960,#15961,#15962,#15963,#15964,#15965,#15966,#15967,#15968,#15969,#15970,
#15971,#15972,#15973,#15974,#15975,#15976,#15977,#15978,#15979,#15980,#15981,
#15982,#15983,#15984,#15985,#15986,#15987,#15988,#15989,#15990,#15991,#15992,
#15993,#15994,#15995,#15996,#15997,#15998,#15999,#16000,#16001,#16002,#16003,
#16004,#16005,#16006,#16007,#16008,#16009,#16010,#16011,#16012,#16013,#16014,
#16015,#16016,#16017,#16018,#16019,#16020,#16021,#16022,#16023,#16024,#16025,
#16026)),.UNSPECIFIED.,.F.,.F.,.F.,(4,4),(4,1,1,1,1,1,1,1,1,1,1,1,1,1,1,
1,1,1,1,1,1,1,1,1,1,1,1,1,1,1,1,1,1,1,1,1,1,1,1,1,1,1,1,1,1,1,1,1,1,1,1,
1,1,1,1,1,1,1,1,1,1,1,1,1,1,1,1,1,1,1,1,1,1,1,1,1,1,1,1,1,1,1,1,1,1,1,1,
1,1,1,1,1,1,1,1,1,1,1,1,1,1,1,1,1,1,1,1,1,1,1,1,1,1,1,1,1,1,1,1,1,1,1,1,
1,1,1,1,1,1,1,1,1,1,1,1,1,1,1,1,1,1,1,1,1,1,1,1,1,1,1,1,1,1,1,1,1,1,1,1,
1,1,1,1,1,1,1,1,1,1,1,1,1,1,1,1,1,1,1,1,1,1,1,1,1,1,1,1,1,1,1,1,1,1,4),
(0.,0.0329955678841871),(11.6159397475006,12.61358260836,13.6112254692194,
14.6088683300789,15.6065111909383,16.6041540517977,17.6017969126571,18.5994397735165,
19.5970826343759,20.5947254952353,21.5923683560947,22.5900112169541,23.5876540778135,
24.5852969386729,25.5829397995323,26.5805826603917,27.5782255212511,28.5758683821105,
29.5735112429699,30.5711541038294,31.5687969646888,32.5664398255482,33.5640826864076,
34.561725547267,35.5593684081264,36.5570112689858,37.5546541298452,38.5522969907046,
39.549939851564,40.5475827124234,41.5452255732828,42.5428684341422,43.5405112950016,
44.538154155861,45.5357970167204,46.5334398775799,47.5310827384393,48.5287255992987,
49.5263684601581,50.5240113210175,51.5216541818769,52.5192970427363,53.5169399035957,
54.5145827644551,55.5122256253145,56.5098684861739,57.5075113470333,58.5051542078927,
59.5027970687521,60.5004399296115,61.4980827904709,62.4957256513303,63.4933685121897,
64.4910113730492,65.4886542339086,66.486297094768,67.4839399556274,68.4815828164868,
69.4792256773462,70.4768685382056,71.474511399065,72.4721542599244,73.4697971207838,
74.4674399816432,75.4650828425026,76.462725703362,77.4603685642214,78.4580114250808,
79.4556542859402,80.4532971467996,81.4509400076591,82.4485828685185,83.4462257293779,
84.4438685902373,85.4415114510967,86.4391543119561,87.4367971728155,88.4344400336749,
89.4320828945343,90.4297257553937,91.4273686162531,92.4250114771125,93.4226543379719,
94.4202971988313,95.4179400596907,96.4155829205502,97.4132257814096,98.410868642269,
99.4085115031284,100.406154363988,101.403797224847,102.401440085707,103.399082946566,
104.396725807425,105.394368668285,106.392011529144,107.389654390004,108.387297250863,
109.384940111722,110.382582972582,111.380225833441,112.377868694301,113.37551155516,
114.373154416019,115.370797276879,116.368440137738,117.366082998598,118.363725859457,
119.361368720316,120.359011581176,121.356654442035,122.354297302895,123.351940163754,
124.349583024614,125.347225885473,126.344868746332,127.342511607192,128.340154468051,
129.337797328911,130.33544018977,131.333083050629,132.330725911489,133.328368772348,
134.326011633208,135.323654494067,136.321297354926,137.318940215786,138.316583076645,
139.314225937505,140.311868798364,141.309511659223,142.307154520083,143.304797380942,
144.302440241802,145.300083102661,146.29772596352,147.29536882438,148.293011685239,
149.290654546099,150.288297406958,151.285940267817,152.283583128677,153.281225989536,
154.278868850396,155.276511711255,156.274154572115,157.271797432974,158.269440293833,
159.267083154693,160.264726015552,161.262368876412,162.260011737271,163.25765459813,
164.25529745899,165.252940319849,166.250583180709,167.248226041568,168.245868902427,
169.243511763287,170.241154624146,171.238797485006,172.236440345865,173.234083206724,
174.231726067584,175.229368928443,176.227011789303,177.224654650162,178.222297511021,
179.219940371881,180.21758323274,181.2152260936,182.212868954459,183.210511815318,
184.208154676178,185.205797537037,186.203440397897,187.201083258756,188.198726119616,
189.196368980475,190.194011841334,191.191654702194,192.189297563053,193.186940423913,
194.184583284772,195.182226145631,196.179869006491,197.17751186735,198.17515472821,
199.172797589069,200.170440449928,201.168083310788,202.165726171647,203.163369032507,
204.161011893366),.UNSPECIFIED.);
#157=B_SPLINE_SURFACE_WITH_KNOTS('',3,3,((#16116,#16117,#16118,#16119,#16120,
#16121,#16122,#16123,#16124,#16125,#16126,#16127,#16128,#16129,#16130,#16131,
#16132,#16133,#16134,#16135,#16136,#16137,#16138,#16139,#16140,#16141,#16142,
#16143,#16144,#16145,#16146,#16147,#16148,#16149,#16150,#16151,#16152,#16153,
#16154,#16155,#16156,#16157,#16158,#16159,#16160,#16161,#16162,#16163,#16164,
#16165,#16166,#16167,#16168,#16169,#16170,#16171,#16172,#16173,#16174,#16175,
#16176,#16177,#16178,#16179,#16180,#16181,#16182,#16183,#16184,#16185,#16186,
#16187,#16188,#16189,#16190,#16191,#16192,#16193,#16194,#16195,#16196,#16197,
#16198,#16199,#16200,#16201,#16202,#16203,#16204,#16205,#16206,#16207,#16208,
#16209,#16210,#16211,#16212,#16213,#16214,#16215,#16216,#16217,#16218,#16219,
#16220,#16221,#16222,#16223,#16224,#16225,#16226,#16227,#16228,#16229,#16230,
#16231,#16232,#16233,#16234,#16235,#16236,#16237,#16238,#16239,#16240,#16241,
#16242,#16243,#16244,#16245,#16246,#16247,#16248,#16249,#16250,#16251,#16252,
#16253,#16254,#16255,#16256,#16257,#16258,#16259,#16260,#16261,#16262,#16263,
#16264,#16265,#16266,#16267,#16268,#16269,#16270,#16271,#16272,#16273,#16274,
#16275,#16276,#16277,#16278,#16279,#16280,#16281,#16282,#16283,#16284,#16285,
#16286,#16287,#16288,#16289,#16290,#16291,#16292,#16293,#16294,#16295,#16296,
#16297,#16298,#16299,#16300,#16301,#16302,#16303,#16304,#16305,#16306,#16307,
#16308,#16309,#16310,#16311,#16312,#16313),(#16314,#16315,#16316,#16317,
#16318,#16319,#16320,#16321,#16322,#16323,#16324,#16325,#16326,#16327,#16328,
#16329,#16330,#16331,#16332,#16333,#16334,#16335,#16336,#16337,#16338,#16339,
#16340,#16341,#16342,#16343,#16344,#16345,#16346,#16347,#16348,#16349,#16350,
#16351,#16352,#16353,#16354,#16355,#16356,#16357,#16358,#16359,#16360,#16361,
#16362,#16363,#16364,#16365,#16366,#16367,#16368,#16369,#16370,#16371,#16372,
#16373,#16374,#16375,#16376,#16377,#16378,#16379,#16380,#16381,#16382,#16383,
#16384,#16385,#16386,#16387,#16388,#16389,#16390,#16391,#16392,#16393,#16394,
#16395,#16396,#16397,#16398,#16399,#16400,#16401,#16402,#16403,#16404,#16405,
#16406,#16407,#16408,#16409,#16410,#16411,#16412,#16413,#16414,#16415,#16416,
#16417,#16418,#16419,#16420,#16421,#16422,#16423,#16424,#16425,#16426,#16427,
#16428,#16429,#16430,#16431,#16432,#16433,#16434,#16435,#16436,#16437,#16438,
#16439,#16440,#16441,#16442,#16443,#16444,#16445,#16446,#16447,#16448,#16449,
#16450,#16451,#16452,#16453,#16454,#16455,#16456,#16457,#16458,#16459,#16460,
#16461,#16462,#16463,#16464,#16465,#16466,#16467,#16468,#16469,#16470,#16471,
#16472,#16473,#16474,#16475,#16476,#16477,#16478,#16479,#16480,#16481,#16482,
#16483,#16484,#16485,#16486,#16487,#16488,#16489,#16490,#16491,#16492,#16493,
#16494,#16495,#16496,#16497,#16498,#16499,#16500,#16501,#16502,#16503,#16504,
#16505,#16506,#16507,#16508,#16509,#16510,#16511),(#16512,#16513,#16514,
#16515,#16516,#16517,#16518,#16519,#16520,#16521,#16522,#16523,#16524,#16525,
#16526,#16527,#16528,#16529,#16530,#16531,#16532,#16533,#16534,#16535,#16536,
#16537,#16538,#16539,#16540,#16541,#16542,#16543,#16544,#16545,#16546,#16547,
#16548,#16549,#16550,#16551,#16552,#16553,#16554,#16555,#16556,#16557,#16558,
#16559,#16560,#16561,#16562,#16563,#16564,#16565,#16566,#16567,#16568,#16569,
#16570,#16571,#16572,#16573,#16574,#16575,#16576,#16577,#16578,#16579,#16580,
#16581,#16582,#16583,#16584,#16585,#16586,#16587,#16588,#16589,#16590,#16591,
#16592,#16593,#16594,#16595,#16596,#16597,#16598,#16599,#16600,#16601,#16602,
#16603,#16604,#16605,#16606,#16607,#16608,#16609,#16610,#16611,#16612,#16613,
#16614,#16615,#16616,#16617,#16618,#16619,#16620,#16621,#16622,#16623,#16624,
#16625,#16626,#16627,#16628,#16629,#16630,#16631,#16632,#16633,#16634,#16635,
#16636,#16637,#16638,#16639,#16640,#16641,#16642,#16643,#16644,#16645,#16646,
#16647,#16648,#16649,#16650,#16651,#16652,#16653,#16654,#16655,#16656,#16657,
#16658,#16659,#16660,#16661,#16662,#16663,#16664,#16665,#16666,#16667,#16668,
#16669,#16670,#16671,#16672,#16673,#16674,#16675,#16676,#16677,#16678,#16679,
#16680,#16681,#16682,#16683,#16684,#16685,#16686,#16687,#16688,#16689,#16690,
#16691,#16692,#16693,#16694,#16695,#16696,#16697,#16698,#16699,#16700,#16701,
#16702,#16703,#16704,#16705,#16706,#16707,#16708,#16709),(#16710,#16711,
#16712,#16713,#16714,#16715,#16716,#16717,#16718,#16719,#16720,#16721,#16722,
#16723,#16724,#16725,#16726,#16727,#16728,#16729,#16730,#16731,#16732,#16733,
#16734,#16735,#16736,#16737,#16738,#16739,#16740,#16741,#16742,#16743,#16744,
#16745,#16746,#16747,#16748,#16749,#16750,#16751,#16752,#16753,#16754,#16755,
#16756,#16757,#16758,#16759,#16760,#16761,#16762,#16763,#16764,#16765,#16766,
#16767,#16768,#16769,#16770,#16771,#16772,#16773,#16774,#16775,#16776,#16777,
#16778,#16779,#16780,#16781,#16782,#16783,#16784,#16785,#16786,#16787,#16788,
#16789,#16790,#16791,#16792,#16793,#16794,#16795,#16796,#16797,#16798,#16799,
#16800,#16801,#16802,#16803,#16804,#16805,#16806,#16807,#16808,#16809,#16810,
#16811,#16812,#16813,#16814,#16815,#16816,#16817,#16818,#16819,#16820,#16821,
#16822,#16823,#16824,#16825,#16826,#16827,#16828,#16829,#16830,#16831,#16832,
#16833,#16834,#16835,#16836,#16837,#16838,#16839,#16840,#16841,#16842,#16843,
#16844,#16845,#16846,#16847,#16848,#16849,#16850,#16851,#16852,#16853,#16854,
#16855,#16856,#16857,#16858,#16859,#16860,#16861,#16862,#16863,#16864,#16865,
#16866,#16867,#16868,#16869,#16870,#16871,#16872,#16873,#16874,#16875,#16876,
#16877,#16878,#16879,#16880,#16881,#16882,#16883,#16884,#16885,#16886,#16887,
#16888,#16889,#16890,#16891,#16892,#16893,#16894,#16895,#16896,#16897,#16898,
#16899,#16900,#16901,#16902,#16903,#16904,#16905,#16906,#16907)),
 .UNSPECIFIED.,.F.,.F.,.F.,(4,4),(4,1,1,1,1,1,1,1,1,1,1,1,1,1,1,1,1,1,1,
1,1,1,1,1,1,1,1,1,1,1,1,1,1,1,1,1,1,1,1,1,1,1,1,1,1,1,1,1,1,1,1,1,1,1,1,
1,1,1,1,1,1,1,1,1,1,1,1,1,1,1,1,1,1,1,1,1,1,1,1,1,1,1,1,1,1,1,1,1,1,1,1,
1,1,1,1,1,1,1,1,1,1,1,1,1,1,1,1,1,1,1,1,1,1,1,1,1,1,1,1,1,1,1,1,1,1,1,1,
1,1,1,1,1,1,1,1,1,1,1,1,1,1,1,1,1,1,1,1,1,1,1,1,1,1,1,1,1,1,1,1,1,1,1,1,
1,1,1,1,1,1,1,1,1,1,1,1,1,1,1,1,1,1,1,1,1,1,1,1,1,1,1,1,1,1,1,1,4),(0.,
0.0329955678841871),(8.30203615430855,9.30007843543257,10.2981207165566,
11.2961629976806,12.2942052788047,13.2922475599287,14.2902898410527,15.2883321221767,
16.2863744033008,17.2844166844248,18.2824589655488,19.2805012466728,20.2785435277969,
21.2765858089209,22.2746280900449,23.272670371169,24.270712652293,25.268754933417,
26.266797214541,27.2648394956651,28.2628817767891,29.2609240579131,30.2589663390371,
31.2570086201612,32.2550509012852,33.2530931824092,34.2511354635333,35.2491777446573,
36.2472200257813,37.2452623069053,38.2433045880294,39.2413468691534,40.2393891502774,
41.2374314314014,42.2354737125255,43.2335159936495,44.2315582747735,45.2296005558975,
46.2276428370216,47.2256851181456,48.2237273992696,49.2217696803937,50.2198119615177,
51.2178542426417,52.2158965237657,53.2139388048898,54.2119810860138,55.2100233671378,
56.2080656482619,57.2061079293859,58.2041502105099,59.2021924916339,60.200234772758,
61.198277053882,62.196319335006,63.19436161613,64.1924038972541,65.1904461783781,
66.1884884595021,67.1865307406262,68.1845730217502,69.1826153028742,70.1806575839982,
71.1786998651223,72.1767421462463,73.1747844273703,74.1728267084943,75.1708689896184,
76.1689112707424,77.1669535518664,78.1649958329905,79.1630381141145,80.1610803952385,
81.1591226763625,82.1571649574865,83.1552072386106,84.1532495197346,85.1512918008586,
86.1493340819827,87.1473763631067,88.1454186442307,89.1434609253548,90.1415032064788,
91.1395454876028,92.1375877687268,93.1356300498508,94.1336723309749,95.1317146120989,
96.1297568932229,97.127799174347,98.125841455471,99.123883736595,100.121926017719,
101.119968298843,102.118010579967,103.116052861091,104.114095142215,105.112137423339,
106.110179704463,107.108221985587,108.106264266711,109.104306547835,110.102348828959,
111.100391110083,112.098433391207,113.096475672331,114.094517953455,115.092560234579,
116.090602515703,117.088644796828,118.086687077952,119.084729359076,120.0827716402,
121.080813921324,122.078856202448,123.076898483572,124.074940764696,125.07298304582,
126.071025326944,127.069067608068,128.067109889192,129.065152170316,130.06319445144,
131.061236732564,132.059279013688,133.057321294812,134.055363575936,135.05340585706,
136.051448138184,137.049490419308,138.047532700432,139.045574981556,140.04361726268,
141.041659543804,142.039701824928,143.037744106052,144.035786387176,145.0338286683,
146.031870949424,147.029913230548,148.027955511672,149.025997792796,150.02404007392,
151.022082355044,152.020124636168,153.018166917292,154.016209198417,155.014251479541,
156.012293760665,157.010336041789,158.008378322913,159.006420604037,160.004462885161,
161.002505166285,162.000547447409,162.998589728533,163.996632009657,164.994674290781,
165.992716571905,166.990758853029,167.988801134153,168.986843415277,169.984885696401,
170.982927977525,171.980970258649,172.979012539773,173.977054820897,174.975097102021,
175.973139383145,176.971181664269,177.969223945393,178.967266226517,179.965308507641,
180.963350788765,181.961393069889,182.959435351013,183.957477632137,184.955519913261,
185.953562194385,186.951604475509,187.949646756633,188.947689037757,189.945731318881,
190.943773600006,191.94181588113,192.939858162254,193.937900443378,194.935942724502,
195.933985005626,196.93202728675,197.930069567874,198.928111848998,199.926154130122,
200.924196411246,201.92223869237,202.920280973494),.UNSPECIFIED.);
#158=B_SPLINE_SURFACE_WITH_KNOTS('',3,3,((#17366,#17367,#17368,#17369,#17370,
#17371,#17372,#17373,#17374,#17375,#17376,#17377,#17378,#17379,#17380,#17381,
#17382,#17383,#17384,#17385,#17386,#17387,#17388,#17389,#17390,#17391,#17392,
#17393,#17394,#17395,#17396,#17397,#17398,#17399,#17400,#17401),(#17402,
#17403,#17404,#17405,#17406,#17407,#17408,#17409,#17410,#17411,#17412,#17413,
#17414,#17415,#17416,#17417,#17418,#17419,#17420,#17421,#17422,#17423,#17424,
#17425,#17426,#17427,#17428,#17429,#17430,#17431,#17432,#17433,#17434,#17435,
#17436,#17437),(#17438,#17439,#17440,#17441,#17442,#17443,#17444,#17445,
#17446,#17447,#17448,#17449,#17450,#17451,#17452,#17453,#17454,#17455,#17456,
#17457,#17458,#17459,#17460,#17461,#17462,#17463,#17464,#17465,#17466,#17467,
#17468,#17469,#17470,#17471,#17472,#17473),(#17474,#17475,#17476,#17477,
#17478,#17479,#17480,#17481,#17482,#17483,#17484,#17485,#17486,#17487,#17488,
#17489,#17490,#17491,#17492,#17493,#17494,#17495,#17496,#17497,#17498,#17499,
#17500,#17501,#17502,#17503,#17504,#17505,#17506,#17507,#17508,#17509)),
 .UNSPECIFIED.,.F.,.F.,.F.,(4,4),(4,1,1,1,1,1,1,1,1,1,1,1,1,1,1,1,1,1,1,
1,1,1,1,1,1,1,1,1,1,1,1,1,1,4),(0.,0.0321584099938622),(11.8553612635794,
12.830508595889,13.8056559281987,14.7808032605084,15.755950592818,16.7310979251277,
17.7062452574374,18.681392589747,19.6565399220567,20.6316872543664,21.606834586676,
22.5819819189857,23.5571292512954,24.532276583605,25.5074239159147,26.4825712482243,
27.457718580534,28.4328659128437,29.4080132451533,30.383160577463,31.3583079097727,
32.3334552420823,33.308602574392,34.2837499067017,35.2588972390113,36.234044571321,
37.2091919036307,38.1843392359403,39.15948656825,40.1346339005596,41.1097812328693,
42.084928565179,43.0600758974886,44.0352232297983),.UNSPECIFIED.);
#159=B_SPLINE_SURFACE_WITH_KNOTS('',3,3,((#17633,#17634,#17635,#17636,#17637,
#17638,#17639,#17640,#17641,#17642,#17643,#17644,#17645,#17646,#17647,#17648,
#17649,#17650,#17651,#17652,#17653,#17654,#17655,#17656,#17657,#17658,#17659,
#17660,#17661,#17662,#17663,#17664,#17665,#17666,#17667,#17668),(#17669,
#17670,#17671,#17672,#17673,#17674,#17675,#17676,#17677,#17678,#17679,#17680,
#17681,#17682,#17683,#17684,#17685,#17686,#17687,#17688,#17689,#17690,#17691,
#17692,#17693,#17694,#17695,#17696,#17697,#17698,#17699,#17700,#17701,#17702,
#17703,#17704),(#17705,#17706,#17707,#17708,#17709,#17710,#17711,#17712,
#17713,#17714,#17715,#17716,#17717,#17718,#17719,#17720,#17721,#17722,#17723,
#17724,#17725,#17726,#17727,#17728,#17729,#17730,#17731,#17732,#17733,#17734,
#17735,#17736,#17737,#17738,#17739,#17740),(#17741,#17742,#17743,#17744,
#17745,#17746,#17747,#17748,#17749,#17750,#17751,#17752,#17753,#17754,#17755,
#17756,#17757,#17758,#17759,#17760,#17761,#17762,#17763,#17764,#17765,#17766,
#17767,#17768,#17769,#17770,#17771,#17772,#17773,#17774,#17775,#17776)),
 .UNSPECIFIED.,.F.,.F.,.F.,(4,4),(4,1,1,1,1,1,1,1,1,1,1,1,1,1,1,1,1,1,1,
1,1,1,1,1,1,1,1,1,1,1,1,1,1,4),(0.,0.0321584099938622),(14.3984001269719,
15.3735474592815,16.3486947915912,17.3238421239009,18.2989894562105,19.2741367885202,
20.2492841208299,21.2244314531395,22.1995787854492,23.1747261177589,24.1498734500685,
25.1250207823782,26.1001681146879,27.0753154469975,28.0504627793072,29.0256101116168,
30.0007574439265,30.9759047762362,31.9510521085458,32.9261994408555,33.9013467731652,
34.8764941054748,35.8516414377845,36.8267887700942,37.8019361024038,38.7770834347135,
39.7522307670232,40.7273780993328,41.7025254316425,42.6776727639522,43.6528200962618,
44.6279674285715,45.6031147608811,46.5782620931908),.UNSPECIFIED.);
#160=B_SPLINE_SURFACE_WITH_KNOTS('',3,3,((#18008,#18009,#18010,#18011,#18012),
(#18013,#18014,#18015,#18016,#18017),(#18018,#18019,#18020,#18021,#18022),
(#18023,#18024,#18025,#18026,#18027),(#18028,#18029,#18030,#18031,#18032)),
 .UNSPECIFIED.,.F.,.F.,.F.,(4,1,4),(4,1,4),(0.,0.571428571428571,1.),(0.,
0.0453052401185593,0.105712226943305),.UNSPECIFIED.);
#161=B_SPLINE_SURFACE_WITH_KNOTS('',3,3,((#18055,#18056,#18057,#18058,#18059),
(#18060,#18061,#18062,#18063,#18064),(#18065,#18066,#18067,#18068,#18069),
(#18070,#18071,#18072,#18073,#18074),(#18075,#18076,#18077,#18078,#18079)),
 .UNSPECIFIED.,.F.,.F.,.F.,(4,1,4),(4,1,4),(0.,0.571428571428571,1.),(0.,
0.0453052401439183,0.105712227002476),.UNSPECIFIED.);
#162=B_SPLINE_SURFACE_WITH_KNOTS('',3,3,((#18093,#18094,#18095,#18096,#18097),
(#18098,#18099,#18100,#18101,#18102),(#18103,#18104,#18105,#18106,#18107),
(#18108,#18109,#18110,#18111,#18112),(#18113,#18114,#18115,#18116,#18117)),
 .UNSPECIFIED.,.F.,.F.,.F.,(4,1,4),(4,1,4),(0.,0.571428571428571,1.),(0.,
4.20509945658767,9.8118987320379),.UNSPECIFIED.);
#163=B_SPLINE_SURFACE_WITH_KNOTS('',3,3,((#18131,#18132,#18133,#18134,#18135),
(#18136,#18137,#18138,#18139,#18140),(#18141,#18142,#18143,#18144,#18145),
(#18146,#18147,#18148,#18149,#18150),(#18151,#18152,#18153,#18154,#18155)),
 .UNSPECIFIED.,.F.,.F.,.F.,(4,1,4),(4,1,4),(0.,0.571428571428571,1.),(0.,
0.0444882141544403,0.103805833027027),.UNSPECIFIED.);
#164=B_SPLINE_SURFACE_WITH_KNOTS('',3,3,((#18175,#18176,#18177,#18178,#18179),
(#18180,#18181,#18182,#18183,#18184),(#18185,#18186,#18187,#18188,#18189),
(#18190,#18191,#18192,#18193,#18194),(#18195,#18196,#18197,#18198,#18199)),
 .UNSPECIFIED.,.F.,.F.,.F.,(4,1,4),(4,1,4),(0.,0.571428571428571,1.),(2.06005858395869E-18,
0.0444882141931362,0.103805833117318),.UNSPECIFIED.);
#165=B_SPLINE_SURFACE_WITH_KNOTS('',3,3,((#18213,#18214,#18215,#18216,#18217),
(#18218,#18219,#18220,#18221,#18222),(#18223,#18224,#18225,#18226,#18227),
(#18228,#18229,#18230,#18231,#18232),(#18233,#18234,#18235,#18236,#18237)),
 .UNSPECIFIED.,.F.,.F.,.F.,(4,1,4),(4,1,4),(0.,0.571428571428571,1.),(0.,
4.20509909783593,9.81189789495051),.UNSPECIFIED.);
#166=B_SPLINE_SURFACE_WITH_KNOTS('',3,3,((#18260,#18261,#18262,#18263),
(#18264,#18265,#18266,#18267),(#18268,#18269,#18270,#18271),(#18272,#18273,
#18274,#18275),(#18276,#18277,#18278,#18279)),.UNSPECIFIED.,.F.,.F.,.F.,
(4,1,4),(4,4),(0.,0.571428571428571,1.),(-0.00268702576369722,0.125151053668407),
 .UNSPECIFIED.);
#167=B_SPLINE_SURFACE_WITH_KNOTS('',3,3,((#18313,#18314,#18315,#18316),
(#18317,#18318,#18319,#18320),(#18321,#18322,#18323,#18324),(#18325,#18326,
#18327,#18328)),.UNSPECIFIED.,.F.,.F.,.F.,(4,4),(4,4),(0.0135518988075539,
0.986045335056424),(0.,0.622596671418298),.UNSPECIFIED.);
#168=B_SPLINE_SURFACE_WITH_KNOTS('',3,3,((#18338,#18339,#18340,#18341),
(#18342,#18343,#18344,#18345),(#18346,#18347,#18348,#18349),(#18350,#18351,
#18352,#18353),(#18354,#18355,#18356,#18357)),.UNSPECIFIED.,.F.,.F.,.F.,
(4,1,4),(4,4),(0.,0.571428571428571,1.),(-0.00281084541253883,0.124959300034279),
 .UNSPECIFIED.);
#169=B_SPLINE_SURFACE_WITH_KNOTS('',3,3,((#18399,#18400,#18401,#18402),
(#18403,#18404,#18405,#18406),(#18407,#18408,#18409,#18410),(#18411,#18412,
#18413,#18414),(#18415,#18416,#18417,#18418)),.UNSPECIFIED.,.F.,.F.,.F.,
(4,1,4),(4,4),(0.,0.571428571428571,1.),(-0.00261432509268751,0.125151053668407),
 .UNSPECIFIED.);
#170=B_SPLINE_SURFACE_WITH_KNOTS('',3,3,((#18452,#18453,#18454,#18455),
(#18456,#18457,#18458,#18459),(#18460,#18461,#18462,#18463),(#18464,#18465,
#18466,#18467),(#18468,#18469,#18470,#18471)),.UNSPECIFIED.,.F.,.F.,.F.,
(4,1,4),(4,4),(0.,0.571428571428571,1.),(-0.00286362952972032,0.124959300034279),
 .UNSPECIFIED.);
#171=B_SPLINE_SURFACE_WITH_KNOTS('',3,3,((#18510,#18511,#18512,#18513),
(#18514,#18515,#18516,#18517),(#18518,#18519,#18520,#18521),(#18522,#18523,
#18524,#18525)),.UNSPECIFIED.,.F.,.F.,.F.,(4,4),(4,4),(0.0139546649435754,
0.986448101192446),(0.,0.622596671418299),.UNSPECIFIED.);
#172=B_SPLINE_CURVE_WITH_KNOTS('',3,(#8715,#8716,#8717,#8718,#8719,#8720,
#8721,#8722,#8723,#8724,#8725,#8726,#8727,#8728,#8729,#8730,#8731,#8732,
#8733,#8734,#8735,#8736,#8737,#8738),.UNSPECIFIED.,.F.,.F.,(4,2,2,2,2,2,
2,2,2,2,2,4),(-0.337265338267783,-0.250544943628509,-0.208272806508042,
-0.186542211788094,-0.176382978682897,-0.170925844043069,-0.16639450677335,
-0.161077381235501,-0.15182241135393,-0.115009181549223,-0.030206004227969,
0.),.UNSPECIFIED.);
#173=B_SPLINE_CURVE_WITH_KNOTS('',3,(#8743,#8744,#8745,#8746,#8747,#8748,
#8749,#8750,#8751,#8752,#8753,#8754,#8755,#8756,#8757,#8758,#8759,#8760,
#8761,#8762),.UNSPECIFIED.,.F.,.F.,(4,2,2,2,2,2,2,2,2,4),(-0.240982594686416,
-0.16829976149504,-0.141836598208813,-0.129116059226128,-0.121962912034391,
-0.115857591426886,-0.108506552485159,-0.0948769875819265,-0.0364654790774683,
0.),.UNSPECIFIED.);
#174=B_SPLINE_CURVE_WITH_KNOTS('',3,(#8767,#8768,#8769,#8770,#8771,#8772,
#8773,#8774,#8775,#8776,#8777,#8778,#8779,#8780,#8781,#8782,#8783,#8784,
#8785,#8786),.UNSPECIFIED.,.F.,.F.,(4,2,2,2,2,2,2,2,2,4),(-0.240981214998207,
-0.168303541671295,-0.141841407502325,-0.129121097580905,-0.121968013294536,
-0.115862708924237,-0.108511643765797,-0.0948818976588229,-0.0364681276985956,
0.),.UNSPECIFIED.);
#175=B_SPLINE_CURVE_WITH_KNOTS('',3,(#8791,#8792,#8793,#8794,#8795,#8796,
#8797,#8798,#8799,#8800,#8801,#8802,#8803,#8804,#8805,#8806,#8807,#8808,
#8809,#8810,#8811,#8812,#8813,#8814),.UNSPECIFIED.,.F.,.F.,(4,2,2,2,2,2,
2,2,2,2,2,4),(-0.337269388373684,-0.250545316912909,-0.208282401844766,
-0.186554569827561,-0.176396213396297,-0.17093921790305,-0.16640782243471,
-0.161090427650893,-0.151834477986603,-0.115010808423941,-0.0302102096065556,
0.),.UNSPECIFIED.);
#176=B_SPLINE_CURVE_WITH_KNOTS('',3,(#8837,#8838,#8839,#8840),
 .UNSPECIFIED.,.F.,.F.,(4,4),(1.0454440030657,2.52465537163019),
 .UNSPECIFIED.);
#177=B_SPLINE_CURVE_WITH_KNOTS('',3,(#8842,#8843,#8844,#8845,#8846,#8847,
#8848,#8849,#8850,#8851,#8852,#8853,#8854,#8855,#8856,#8857,#8858,#8859,
#8860,#8861,#8862,#8863,#8864,#8865,#8866,#8867,#8868,#8869),
 .UNSPECIFIED.,.F.,.F.,(4,3,3,3,3,3,3,3,3,4),(-0.152193408756968,-0.128427023368412,
-0.115107736263918,-0.0911810900745799,-0.0780377802127556,-0.0652031397886901,
-0.0414031558437525,-0.0389949527774582,-0.0152076153333754,0.),
 .UNSPECIFIED.);
#178=B_SPLINE_CURVE_WITH_KNOTS('',3,(#8871,#8872,#8873,#8874),
 .UNSPECIFIED.,.F.,.F.,(4,4),(-3.44967454744645,-1.05170160817356),
 .UNSPECIFIED.);
#179=B_SPLINE_CURVE_WITH_KNOTS('',3,(#8876,#8877,#8878,#8879,#8880,#8881,
#8882,#8883,#8884,#8885,#8886,#8887,#8888,#8889,#8890,#8891,#8892,#8893,
#8894,#8895,#8896,#8897,#8898,#8899,#8900,#8901,#8902,#8903),
 .UNSPECIFIED.,.F.,.F.,(4,3,3,3,3,3,3,3,3,4),(-0.152278960443096,-0.128503570101575,
-0.115218572146868,-0.09145408274965,-0.0870214650669139,-0.0781562978024333,
-0.0542566895399357,-0.03908030849237,-0.0153296112319379,0.),
 .UNSPECIFIED.);
#180=B_SPLINE_CURVE_WITH_KNOTS('',3,(#8904,#8905,#8906,#8907),
 .UNSPECIFIED.,.F.,.F.,(4,4),(2.75501813708031,3.4476340663212),
 .UNSPECIFIED.);
#181=B_SPLINE_CURVE_WITH_KNOTS('',3,(#8929,#8930,#8931,#8932),
 .UNSPECIFIED.,.F.,.F.,(4,4),(7.24810383506675,7.89761558728778),
 .UNSPECIFIED.);
#182=B_SPLINE_CURVE_WITH_KNOTS('',3,(#8934,#8935,#8936,#8937,#8938,#8939,
#8940,#8941,#8942,#8943,#8944,#8945,#8946,#8947,#8948,#8949,#8950,#8951,
#8952,#8953,#8954,#8955,#8956,#8957,#8958,#8959,#8960,#8961),
 .UNSPECIFIED.,.F.,.F.,(4,3,3,3,3,3,3,3,3,4),(-0.152278869104567,-0.128548794904564,
-0.115192257893812,-0.0912773536606376,-0.0781090575823055,-0.0652724057916263,
-0.0414819581560496,-0.0390493575290778,-0.015259721743698,0.),
 .UNSPECIFIED.);
#183=B_SPLINE_CURVE_WITH_KNOTS('',3,(#8963,#8964,#8965,#8966),
 .UNSPECIFIED.,.F.,.F.,(4,4),(-9.94532343034734,-7.24519303641511),
 .UNSPECIFIED.);
#184=B_SPLINE_CURVE_WITH_KNOTS('',3,(#8968,#8969,#8970,#8971,#8972,#8973,
#8974,#8975,#8976,#8977,#8978,#8979,#8980,#8981,#8982,#8983,#8984,#8985,
#8986,#8987,#8988,#8989,#8990,#8991,#8992,#8993,#8994,#8995),
 .UNSPECIFIED.,.F.,.F.,(4,3,3,3,3,3,3,3,3,4),(-0.152181623618259,-0.128410404494075,
-0.115248188224843,-0.0914746846046984,-0.0869904866333268,-0.0783028696190655,
-0.0543945376065823,-0.0391651209697638,-0.0153884182770307,0.),
 .UNSPECIFIED.);
#185=B_SPLINE_CURVE_WITH_KNOTS('',3,(#8996,#8997,#8998,#8999),
 .UNSPECIFIED.,.F.,.F.,(4,4),(8.21380824320284,9.95046871680089),
 .UNSPECIFIED.);
#186=B_SPLINE_CURVE_WITH_KNOTS('',3,(#9002,#9003,#9004,#9005),
 .UNSPECIFIED.,.F.,.F.,(4,4),(2.80491490332713,3.45442665446657),
 .UNSPECIFIED.);
#187=B_SPLINE_CURVE_WITH_KNOTS('',3,(#9009,#9010,#9011,#9012),
 .UNSPECIFIED.,.F.,.F.,(4,4),(0.752061768057538,2.48872224644044),
 .UNSPECIFIED.);
#188=B_SPLINE_CURVE_WITH_KNOTS('',3,(#9160,#9161,#9162,#9163,#9164,#9165),
 .UNSPECIFIED.,.F.,.F.,(4,2,4),(-0.606700505977711,-0.303383635264422,-0.000339350725729326),
 .UNSPECIFIED.);
#189=B_SPLINE_CURVE_WITH_KNOTS('',3,(#9166,#9167,#9168,#9169,#9170,#9171,
#9172,#9173,#9174,#9175,#9176,#9177,#9178,#9179,#9180,#9181,#9182,#9183,
#9184,#9185,#9186,#9187,#9188,#9189,#9190,#9191,#9192,#9193),
 .UNSPECIFIED.,.F.,.F.,(4,3,3,3,3,3,3,3,3,4),(-0.152173579228948,-0.128423230539522,
-0.115115104157663,-0.0911927259648815,-0.0780672068328041,-0.0652082609452843,
-0.0414117413801899,-0.0390174000215468,-0.0152300060615686,0.),
 .UNSPECIFIED.);
#190=B_SPLINE_CURVE_WITH_KNOTS('',3,(#9194,#9195,#9196,#9197,#9198,#9199),
 .UNSPECIFIED.,.F.,.F.,(4,2,4),(-0.606471894652381,-0.303383500305553,-0.00011071898471493),
 .UNSPECIFIED.);
#191=B_SPLINE_CURVE_WITH_KNOTS('',3,(#9203,#9204,#9205,#9206,#9207,#9208),
 .UNSPECIFIED.,.F.,.F.,(4,2,4),(-0.606240625011114,-0.303433113375332,-0.00010938105916114),
 .UNSPECIFIED.);
#192=B_SPLINE_CURVE_WITH_KNOTS('',3,(#9210,#9211,#9212,#9213,#9214,#9215,
#9216,#9217,#9218,#9219,#9220,#9221,#9222,#9223,#9224,#9225,#9226,#9227,
#9228,#9229,#9230,#9231,#9232,#9233,#9234,#9235,#9236,#9237),
 .UNSPECIFIED.,.F.,.F.,(4,3,3,3,3,3,3,3,3,4),(-0.152281454644235,-0.128508102092242,
-0.115234945630277,-0.0914677943501604,-0.0870276017853555,-0.0781846052914712,
-0.0542821334115454,-0.0390966859411886,-0.0153419673568312,0.),
 .UNSPECIFIED.);
#193=B_SPLINE_CURVE_WITH_KNOTS('',3,(#9239,#9240,#9241,#9242,#9243,#9244),
 .UNSPECIFIED.,.F.,.F.,(4,2,4),(-0.606758573154242,-0.303433157101101,-0.000627306481538803),
 .UNSPECIFIED.);
#194=B_SPLINE_CURVE_WITH_KNOTS('',3,(#9250,#9251,#9252,#9253,#9254,#9255),
 .UNSPECIFIED.,.F.,.F.,(4,2,4),(-0.60617382748,-0.303436117212405,-7.2700296824213E-5),
 .UNSPECIFIED.);
#195=B_SPLINE_CURVE_WITH_KNOTS('',3,(#9257,#9258,#9259,#9260,#9261,#9262,
#9263,#9264,#9265,#9266,#9267,#9268,#9269,#9270,#9271,#9272,#9273,#9274,
#9275,#9276,#9277,#9278,#9279,#9280,#9281,#9282,#9283,#9284),
 .UNSPECIFIED.,.F.,.F.,(4,3,3,3,3,3,3,3,3,4),(-0.152282154327755,-0.128558036203745,
-0.115201429639692,-0.0912891813973639,-0.0781219052297615,-0.065279687589213,
-0.0414913146723999,-0.0390591331507366,-0.0152683745546824,0.),
 .UNSPECIFIED.);
#196=B_SPLINE_CURVE_WITH_KNOTS('',3,(#9288,#9289,#9290,#9291,#9292,#9293,
#9294,#9295,#9296,#9297,#9298,#9299,#9300,#9301,#9302,#9303,#9304,#9305,
#9306,#9307,#9308,#9309,#9310,#9311,#9312,#9313,#9314,#9315),
 .UNSPECIFIED.,.F.,.F.,(4,3,3,3,3,3,3,3,3,4),(-0.152283066055976,-0.128508717930245,
-0.115216472798554,-0.091451700383826,-0.087022506454752,-0.0781485278686168,
-0.0542483994686567,-0.0390758108455304,-0.0153274175274101,0.),
 .UNSPECIFIED.);
#197=B_SPLINE_CURVE_WITH_KNOTS('',3,(#9317,#9318,#9319,#9320,#9321,#9322),
 .UNSPECIFIED.,.F.,.F.,(4,2,4),(-0.606800264911061,-0.303436147592132,-0.000699137727853738),
 .UNSPECIFIED.);
#198=B_SPLINE_CURVE_WITH_KNOTS('',3,(#9327,#9328,#9329,#9330,#9331,#9332),
 .UNSPECIFIED.,.F.,.F.,(4,2,4),(-0.606915279655722,-0.30363236403835,-0.000516487074480598),
 .UNSPECIFIED.);
#199=B_SPLINE_CURVE_WITH_KNOTS('',3,(#9336,#9337,#9338,#9339,#9340,#9341,
#9342,#9343,#9344,#9345,#9346,#9347,#9348,#9349,#9350,#9351,#9352,#9353,
#9354,#9355,#9356,#9357,#9358,#9359,#9360,#9361,#9362,#9363),
 .UNSPECIFIED.,.F.,.F.,(4,3,3,3,3,3,3,3,3,4),(-0.152205325335401,-0.128433618138404,
-0.115304790388008,-0.091527299141506,-0.0870178586418932,-0.0783866443643876,
-0.0544751548276533,-0.0392137310602028,-0.0154203878854647,0.),
 .UNSPECIFIED.);
#200=B_SPLINE_CURVE_WITH_KNOTS('',3,(#9365,#9366,#9367,#9368,#9369,#9370),
 .UNSPECIFIED.,.F.,.F.,(4,2,4),(-0.606752424187958,-0.303632696349781,-0.000353591088346872),
 .UNSPECIFIED.);
#201=B_SPLINE_CURVE_WITH_KNOTS('',3,(#9376,#9377,#9378,#9379),
 .UNSPECIFIED.,.F.,.F.,(4,4),(0.0116023361771303,0.618489359031386),
 .UNSPECIFIED.);
#202=B_SPLINE_CURVE_WITH_KNOTS('',3,(#9383,#9384,#9385,#9386),
 .UNSPECIFIED.,.F.,.F.,(4,4),(-0.618489359031386,-0.01160233617713),
 .UNSPECIFIED.);
#203=B_SPLINE_CURVE_WITH_KNOTS('',3,(#9389,#9390,#9391,#9392),
 .UNSPECIFIED.,.F.,.F.,(4,4),(7.01593971618694,9.71770560667459),
 .UNSPECIFIED.);
#204=B_SPLINE_CURVE_WITH_KNOTS('',3,(#9393,#9394,#9395,#9396),
 .UNSPECIFIED.,.F.,.F.,(4,4),(0.505945342046796,3.20718651982575),
 .UNSPECIFIED.);
#205=B_SPLINE_CURVE_WITH_KNOTS('',3,(#9399,#9400,#9401,#9402,#9403,#9404,
#9405),.UNSPECIFIED.,.F.,.F.,(4,3,4),(3.40717417387402,5.11170895874517,
6.80746068626633),.UNSPECIFIED.);
#206=B_SPLINE_CURVE_WITH_KNOTS('',3,(#9408,#9409,#9410,#9411),
 .UNSPECIFIED.,.F.,.F.,(4,4),(7.00766573366377,9.41198845520559),
 .UNSPECIFIED.);
#207=B_SPLINE_CURVE_WITH_KNOTS('',3,(#9415,#9416,#9417,#9418),
 .UNSPECIFIED.,.F.,.F.,(4,4),(9.61248784142317,10.2217363065808),
 .UNSPECIFIED.);
#208=B_SPLINE_CURVE_WITH_KNOTS('',3,(#9419,#9420,#9421,#9422,#9423,#9424,
#9425,#9426,#9427,#9428,#9429,#9430,#9431,#9432,#9433,#9434,#9435,#9436,
#9437,#9438,#9439,#9440,#9441,#9442,#9443,#9444,#9445,#9446),
 .UNSPECIFIED.,.F.,.F.,(4,3,3,3,3,3,3,3,3,4),(0.,0.0238103109064959,0.0390781362249314,
0.0628635086275546,0.0641230352384255,0.0780643700703951,0.101962174814111,
0.113803522271848,0.137549611554782,0.149564734365165),.UNSPECIFIED.);
#209=B_SPLINE_CURVE_WITH_KNOTS('',3,(#9450,#9451,#9452,#9453,#9454,#9455,
#9456,#9457,#9458,#9459,#9460,#9461,#9462,#9463,#9464,#9465,#9466,#9467,
#9468,#9469,#9470,#9471,#9472,#9473,#9474,#9475,#9476,#9477,#9478,#9479,
#9480),.UNSPECIFIED.,.F.,.F.,(4,3,3,3,3,3,3,3,3,3,4),(0.,0.0535521515156599,
0.107729685495911,0.117233338918226,0.171447998942947,0.1923696899792,0.234191611538245,
0.288659693466396,0.341410301570312,0.395549383747909,0.448696573746633),
 .UNSPECIFIED.);
#210=B_SPLINE_CURVE_WITH_KNOTS('',3,(#9482,#9483,#9484,#9485),
 .UNSPECIFIED.,.F.,.F.,(4,4),(0.0255858263485814,0.973760737485873),
 .UNSPECIFIED.);
#211=B_SPLINE_CURVE_WITH_KNOTS('',3,(#9487,#9488,#9489,#9490,#9491,#9492,
#9493,#9494,#9495,#9496,#9497,#9498,#9499,#9500,#9501,#9502,#9503,#9504,
#9505,#9506,#9507,#9508,#9509,#9510,#9511,#9512,#9513,#9514,#9515,#9516,
#9517),.UNSPECIFIED.,.F.,.F.,(4,3,3,3,3,3,3,3,3,3,4),(0.,0.0535144560117858,
0.107726856902975,0.117300577410231,0.171517675930231,0.195438847090422,
0.234297456941738,0.289665153342662,0.345032849743585,0.40043206955427,
0.455831289364955),.UNSPECIFIED.);
#212=B_SPLINE_CURVE_WITH_KNOTS('',3,(#9521,#9522,#9523,#9524,#9525,#9526,
#9527,#9528,#9529,#9530,#9531,#9532,#9533,#9534,#9535,#9536,#9537,#9538,
#9539,#9540,#9541,#9542,#9543,#9544,#9545,#9546,#9547,#9548,#9549,#9550,
#9551),.UNSPECIFIED.,.F.,.F.,(4,3,3,3,3,3,3,3,3,3,4),(0.,0.053505543180391,
0.107714168832353,0.117253997025819,0.171473395203321,0.195418854185489,
0.234223199196375,0.289607016015183,0.344990832833991,0.400409777473312,
0.455828722112633),.UNSPECIFIED.);
#213=B_SPLINE_CURVE_WITH_KNOTS('',3,(#9553,#9554,#9555,#9556),
 .UNSPECIFIED.,.F.,.F.,(4,4),(0.0262392625141271,0.974414173651419),
 .UNSPECIFIED.);
#214=B_SPLINE_CURVE_WITH_KNOTS('',3,(#9558,#9559,#9560,#9561,#9562,#9563,
#9564,#9565,#9566,#9567,#9568,#9569,#9570,#9571,#9572,#9573,#9574,#9575,
#9576,#9577,#9578,#9579,#9580,#9581,#9582,#9583,#9584,#9585,#9586,#9587,
#9588),.UNSPECIFIED.,.F.,.F.,(4,3,3,3,3,3,3,3,3,3,4),(0.,0.0535648734523888,
0.107747221190676,0.117299947751206,0.171510987106922,0.192397607227928,
0.234296687348373,0.288768001369001,0.341469499352622,0.395597672314973,
0.448700135162036),.UNSPECIFIED.);
#215=B_SPLINE_CURVE_WITH_KNOTS('',3,(#9591,#9592,#9593,#9594,#9595,#9596,
#9597,#9598,#9599,#9600,#9601,#9602,#9603,#9604,#9605,#9606,#9607,#9608,
#9609,#9610,#9611,#9612,#9613,#9614,#9615),.UNSPECIFIED.,.F.,.F.,(4,3,3,
3,3,3,3,3,4),(0.,0.0238141989470671,0.0391004231578824,0.0641320992313133,
0.0780996136084711,0.101998806889826,0.113823260594808,0.137564745199532,
0.149565921982294),.UNSPECIFIED.);
#216=B_SPLINE_CURVE_WITH_KNOTS('',3,(#9617,#9618,#9619,#9620),
 .UNSPECIFIED.,.F.,.F.,(4,4),(2.76692059912875E-5,0.609394470571143),
 .UNSPECIFIED.);
#217=B_SPLINE_CURVE_WITH_KNOTS('',3,(#9623,#9624,#9625,#9626),
 .UNSPECIFIED.,.F.,.F.,(4,4),(0.809932799154201,3.21472245120952),
 .UNSPECIFIED.);
#218=B_SPLINE_CURVE_WITH_KNOTS('',3,(#9629,#9630,#9631,#9632,#9633,#9634,
#9635),.UNSPECIFIED.,.F.,.F.,(4,3,4),(3.41496637450242,5.11093193409745,
6.81591321610411),.UNSPECIFIED.);
#219=B_SPLINE_CURVE_WITH_KNOTS('',3,(#9639,#9640,#9641,#9642),
 .UNSPECIFIED.,.F.,.F.,(4,4),(9.91798263530139,10.2237206759544),
 .UNSPECIFIED.);
#220=B_SPLINE_CURVE_WITH_KNOTS('',3,(#9644,#9645,#9646,#9647,#9648,#9649,
#9650,#9651,#9652,#9653,#9654,#9655,#9656,#9657,#9658,#9659,#9660,#9661,
#9662,#9663,#9664,#9665,#9666,#9667,#9668,#9669,#9670,#9671),
 .UNSPECIFIED.,.F.,.F.,(4,3,3,3,3,3,3,3,3,4),(0.,0.023807020713713,0.039085080816122,
0.0628703378723092,0.0651394887354207,0.0780750047750988,0.101981498769656,
0.114997221725907,0.138748569029605,0.151942344104828),.UNSPECIFIED.);
#221=B_SPLINE_CURVE_WITH_KNOTS('',3,(#9675,#9676,#9677,#9678,#9679,#9680,
#9681,#9682,#9683,#9684,#9685,#9686,#9687,#9688,#9689,#9690,#9691,#9692,
#9693,#9694,#9695,#9696,#9697,#9698,#9699,#9700,#9701,#9702),
 .UNSPECIFIED.,.F.,.F.,(4,3,3,3,3,3,3,3,3,4),(0.,0.0238098191818892,0.0391006681981376,
0.0628849269680955,0.0651459659463291,0.0780999162396042,0.102007524384594,
0.115011225379555,0.138759376430353,0.151943200125079),.UNSPECIFIED.);
#222=B_SPLINE_CURVE_WITH_KNOTS('',3,(#9704,#9705,#9706,#9707),
 .UNSPECIFIED.,.F.,.F.,(4,4),(2.85486020485948E-5,0.305707210239178),
 .UNSPECIFIED.);
#223=B_SPLINE_CURVE_WITH_KNOTS('',3,(#9717,#9718,#9719,#9720,#9721,#9722),
 .UNSPECIFIED.,.F.,.F.,(4,2,4),(-0.606446248197249,-0.303383959626182,-6.4365448350312E-5),
 .UNSPECIFIED.);
#224=B_SPLINE_CURVE_WITH_KNOTS('',3,(#9724,#9725,#9726,#9727,#9728,#9729),
 .UNSPECIFIED.,.F.,.F.,(4,2,4),(-0.60675170080159,-0.303384112192838,-0.000369837888147484),
 .UNSPECIFIED.);
#225=B_SPLINE_CURVE_WITH_KNOTS('',3,(#9731,#9732,#9733,#9734,#9735,#9736,
#9737,#9738,#9739,#9740,#9741,#9742,#9743,#9744,#9745,#9746,#9747,#9748,
#9749,#9750,#9751,#9752,#9753,#9754,#9755,#9756,#9757,#9758),
 .UNSPECIFIED.,.F.,.F.,(4,3,3,3,3,3,3,3,3,4),(-0.152162866344201,-0.128411131698784,
-0.115108013904405,-0.0911850729173883,-0.0780642464630149,-0.0652023242402653,
-0.0414053499882389,-0.0390151293250392,-0.0152279490549848,0.),
 .UNSPECIFIED.);
#226=B_SPLINE_CURVE_WITH_KNOTS('',3,(#9761,#9762,#9763,#9764,#9765,#9766,
#9767,#9768,#9769,#9770,#9771,#9772,#9773,#9774,#9775,#9776,#9777,#9778,
#9779,#9780,#9781,#9782,#9783,#9784,#9785,#9786,#9787,#9788),
 .UNSPECIFIED.,.F.,.F.,(4,3,3,3,3,3,3,3,3,4),(-0.152171297476962,-0.128400300768352,
-0.115247520946962,-0.0914735511738372,-0.0869860114952295,-0.0783112904282795,
-0.0544025203706761,-0.0391699941254272,-0.015391764586027,0.),
 .UNSPECIFIED.);
#227=B_SPLINE_CURVE_WITH_KNOTS('',3,(#9805,#9806,#9807,#9808),
 .UNSPECIFIED.,.F.,.F.,(4,4),(-3.45733745322815,-0.757207059295936),
 .UNSPECIFIED.);
#228=B_SPLINE_CURVE_WITH_KNOTS('',3,(#9826,#9827,#9828,#9829),
 .UNSPECIFIED.,.F.,.F.,(4,4),(-0.557056952888827,-0.283259008618247),
 .UNSPECIFIED.);
#229=B_SPLINE_CURVE_WITH_KNOTS('',3,(#9830,#9831,#9832,#9833),
 .UNSPECIFIED.,.F.,.F.,(4,4),(-0.618164468641375,-0.0110156167597059),
 .UNSPECIFIED.);
#230=B_SPLINE_CURVE_WITH_KNOTS('',3,(#9875,#9876,#9877,#9878),
 .UNSPECIFIED.,.F.,.F.,(4,4),(0.283259011433088,0.551788488929761),
 .UNSPECIFIED.);
#231=B_SPLINE_CURVE_WITH_KNOTS('',3,(#9882,#9883,#9884,#9885),
 .UNSPECIFIED.,.F.,.F.,(4,4),(10.1507419987596,10.419271481025),
 .UNSPECIFIED.);
#232=B_SPLINE_CURVE_WITH_KNOTS('',3,(#9920,#9921,#9922,#9923),
 .UNSPECIFIED.,.F.,.F.,(4,4),(0.0110156167597055,0.618164468641375),
 .UNSPECIFIED.);
#233=B_SPLINE_CURVE_WITH_KNOTS('',3,(#9924,#9925,#9926,#9927),
 .UNSPECIFIED.,.F.,.F.,(4,4),(-10.419271481025,-10.1454735367545),
 .UNSPECIFIED.);
#234=B_SPLINE_CURVE_WITH_KNOTS('',3,(#9930,#9931,#9932,#9933,#9934,#9935),
 .UNSPECIFIED.,.F.,.F.,(4,2,4),(-0.606211482799139,-0.303431960476852,-9.19895310989571E-5),
 .UNSPECIFIED.);
#235=B_SPLINE_CURVE_WITH_KNOTS('',3,(#9937,#9938,#9939,#9940,#9941,#9942,
#9943,#9944,#9945,#9946,#9947,#9948,#9949,#9950,#9951,#9952,#9953,#9954,
#9955,#9956,#9957,#9958,#9959,#9960,#9961,#9962,#9963,#9964),
 .UNSPECIFIED.,.F.,.F.,(4,3,3,3,3,3,3,3,3,4),(-0.152283340966725,-0.128554242174982,
-0.115196092098682,-0.0912819860997417,-0.0781117853096875,-0.0652755629514801,
-0.0414857317972147,-0.039051434275634,-0.0152612146291672,0.),
 .UNSPECIFIED.);
#236=B_SPLINE_CURVE_WITH_KNOTS('',3,(#9968,#9969,#9970,#9971,#9972,#9973,
#9974,#9975,#9976,#9977,#9978,#9979,#9980,#9981,#9982,#9983,#9984,#9985,
#9986,#9987,#9988,#9989,#9990,#9991,#9992,#9993,#9994,#9995),
 .UNSPECIFIED.,.F.,.F.,(4,3,3,3,3,3,3,3,3,4),(-0.152285570909379,-0.128511627155755,
-0.115232904621082,-0.0914664612111958,-0.0870286654075453,-0.0781769338106538,
-0.0542752301960614,-0.039092246575741,-0.0153386136911565,0.),
 .UNSPECIFIED.);
#237=B_SPLINE_CURVE_WITH_KNOTS('',3,(#9996,#9997,#9998,#9999,#10000,#10001),
 .UNSPECIFIED.,.F.,.F.,(4,2,4),(-0.606773318344362,-0.303431998667662,-0.000653802131222458),
 .UNSPECIFIED.);
#238=B_SPLINE_CURVE_WITH_KNOTS('',3,(#10018,#10019,#10020,#10021),
 .UNSPECIFIED.,.F.,.F.,(4,4),(-7.05313168653828,-3.6572084986735),
 .UNSPECIFIED.);
#239=B_SPLINE_CURVE_WITH_KNOTS('',3,(#10042,#10043,#10044,#10045),
 .UNSPECIFIED.,.F.,.F.,(4,4),(3.65450559744172,7.0548588409572),
 .UNSPECIFIED.);
#240=B_SPLINE_CURVE_WITH_KNOTS('',3,(#10047,#10048,#10049,#10050),
 .UNSPECIFIED.,.F.,.F.,(4,4),(3.64767164868607,7.04802489220155),
 .UNSPECIFIED.);
#241=B_SPLINE_CURVE_WITH_KNOTS('',3,(#10071,#10072,#10073,#10074),
 .UNSPECIFIED.,.F.,.F.,(4,4),(-7.04532199096977,-3.64939880310499),
 .UNSPECIFIED.);
#242=B_SPLINE_CURVE_WITH_KNOTS('',3,(#10093,#10094,#10095,#10096,#10097,
#10098),.UNSPECIFIED.,.F.,.F.,(4,2,4),(-0.606200453641641,-0.30343602424441,
-9.0120313562092E-5),.UNSPECIFIED.);
#243=B_SPLINE_CURVE_WITH_KNOTS('',3,(#10100,#10101,#10102,#10103,#10104,
#10105,#10106,#10107,#10108,#10109,#10110,#10111,#10112,#10113,#10114,#10115,
#10116,#10117,#10118,#10119,#10120,#10121,#10122,#10123,#10124,#10125,#10126,
#10127),.UNSPECIFIED.,.F.,.F.,(4,3,3,3,3,3,3,3,3,4),(-0.152277688086818,
-0.128551334178815,-0.115197577176818,-0.0912856014461669,-0.0781191417238373,
-0.0652765169533013,-0.0414883027365163,-0.0390570310290822,-0.0152653090895913,
0.),.UNSPECIFIED.);
#244=B_SPLINE_CURVE_WITH_KNOTS('',3,(#10129,#10130,#10131,#10132,#10133,
#10134),.UNSPECIFIED.,.F.,.F.,(4,2,4),(-0.60678286609787,-0.303436074842897,
-0.000672492961417026),.UNSPECIFIED.);
#245=B_SPLINE_CURVE_WITH_KNOTS('',3,(#10151,#10152,#10153,#10154),
 .UNSPECIFIED.,.F.,.F.,(4,4),(-9.65082888146972,-7.25285594219682),
 .UNSPECIFIED.);
#246=B_SPLINE_CURVE_WITH_KNOTS('',3,(#10175,#10176,#10177,#10178),
 .UNSPECIFIED.,.F.,.F.,(4,4),(7.25489642332205,7.94751235889625),
 .UNSPECIFIED.);
#247=B_SPLINE_CURVE_WITH_KNOTS('',3,(#10179,#10180,#10181,#10182),
 .UNSPECIFIED.,.F.,.F.,(4,4),(8.17787511801303,9.65708648657758),
 .UNSPECIFIED.);
#248=B_SPLINE_CURVE_WITH_KNOTS('',3,(#10202,#10203,#10204,#10205,#10206,
#10207),.UNSPECIFIED.,.F.,.F.,(4,2,4),(-0.607007797795788,-0.303636495504298,
-0.000571323176327465),.UNSPECIFIED.);
#249=B_SPLINE_CURVE_WITH_KNOTS('',3,(#10209,#10210,#10211,#10212,#10213,
#10214,#10215,#10216,#10217,#10218,#10219,#10220,#10221,#10222,#10223,#10224,
#10225,#10226,#10227,#10228,#10229,#10230,#10231,#10232,#10233,#10234,#10235,
#10236),.UNSPECIFIED.,.F.,.F.,(4,3,3,3,3,3,3,3,3,4),(-0.152184339020145,
-0.128410461444444,-0.115096394428865,-0.0911692948751363,-0.0780261759644403,
-0.0651939085034322,-0.0413932235702045,-0.0389860720679279,-0.0151971168406065,
0.),.UNSPECIFIED.);
#250=B_SPLINE_CURVE_WITH_KNOTS('',3,(#10240,#10241,#10242,#10243,#10244,
#10245,#10246,#10247,#10248,#10249,#10250,#10251,#10252,#10253,#10254,#10255,
#10256,#10257,#10258,#10259,#10260,#10261,#10262,#10263,#10264,#10265,#10266,
#10267),.UNSPECIFIED.,.F.,.F.,(4,3,3,3,3,3,3,3,3,4),(-0.15219777746951,
-0.128424216118147,-0.115318679085322,-0.0915406112613293,-0.0870190514838729,
-0.0784197287877601,-0.0545085386658457,-0.0392329067084975,-0.0154317870320417,
0.),.UNSPECIFIED.);
#251=B_SPLINE_CURVE_WITH_KNOTS('',3,(#10268,#10269,#10270,#10271,#10272,
#10273),.UNSPECIFIED.,.F.,.F.,(4,2,4),(-0.606706256981509,-0.303636876939173,
-0.00026974181288697),.UNSPECIFIED.);
#252=B_SPLINE_CURVE_WITH_KNOTS('',3,(#10291,#10292,#10293,#10294),
 .UNSPECIFIED.,.F.,.F.,(4,4),(0.0112334529114386,0.618489359031386),
 .UNSPECIFIED.);
#253=B_SPLINE_CURVE_WITH_KNOTS('',3,(#10295,#10296,#10297,#10298),
 .UNSPECIFIED.,.F.,.F.,(4,4),(-10.4271318523291,-9.85085636625011),
 .UNSPECIFIED.);
#254=B_SPLINE_CURVE_WITH_KNOTS('',3,(#10321,#10322,#10323,#10324),
 .UNSPECIFIED.,.F.,.F.,(4,4),(9.85750350611301,10.4271318523291),
 .UNSPECIFIED.);
#255=B_SPLINE_CURVE_WITH_KNOTS('',3,(#10328,#10329,#10330,#10331),
 .UNSPECIFIED.,.F.,.F.,(4,4),(0.27539863731415,0.845026983530265),
 .UNSPECIFIED.);
#256=B_SPLINE_CURVE_WITH_KNOTS('',3,(#10349,#10350,#10351,#10352),
 .UNSPECIFIED.,.F.,.F.,(4,4),(-0.851674123393175,-0.27539863731415),
 .UNSPECIFIED.);
#257=B_SPLINE_CURVE_WITH_KNOTS('',3,(#10353,#10354,#10355,#10356),
 .UNSPECIFIED.,.F.,.F.,(4,4),(-0.618489359031386,-0.0112334529114389),
 .UNSPECIFIED.);
#258=B_SPLINE_CURVE_WITH_KNOTS('',3,(#10436,#10437,#10438,#10439),
 .UNSPECIFIED.,.F.,.F.,(4,4),(0.0112755522169305,0.618164468641375),
 .UNSPECIFIED.);
#259=B_SPLINE_CURVE_WITH_KNOTS('',3,(#10460,#10461,#10462,#10463),
 .UNSPECIFIED.,.F.,.F.,(4,4),(-0.618164468641375,-0.0112755522169305),
 .UNSPECIFIED.);
#260=B_SPLINE_CURVE_WITH_KNOTS('',3,(#10549,#10550,#10551,#10552),
 .UNSPECIFIED.,.F.,.F.,(4,4),(5.55111512312578E-17,0.618489359031386),
 .UNSPECIFIED.);
#261=B_SPLINE_CURVE_WITH_KNOTS('',3,(#10553,#10554,#10555,#10556),
 .UNSPECIFIED.,.F.,.F.,(4,4),(-0.618489359031386,-0.00110654915602034),
 .UNSPECIFIED.);
#262=B_SPLINE_CURVE_WITH_KNOTS('',3,(#10592,#10593,#10594,#10595,#10596),
 .UNSPECIFIED.,.F.,.F.,(4,1,4),(-10.4271318523291,-4.63063308449434,-0.283259008618247),
 .UNSPECIFIED.);
#263=B_SPLINE_CURVE_WITH_KNOTS('',3,(#10597,#10598,#10599,#10600,#10601),
 .UNSPECIFIED.,.F.,.F.,(4,1,4),(0.283259011433087,4.63063308449434,10.4271318523291),
 .UNSPECIFIED.);
#264=B_SPLINE_CURVE_WITH_KNOTS('',3,(#10622,#10623,#10624,#10625),
 .UNSPECIFIED.,.F.,.F.,(4,4),(0.000779732613545348,0.618164468641375),
 .UNSPECIFIED.);
#265=B_SPLINE_CURVE_WITH_KNOTS('',3,(#10626,#10627,#10628,#10629),
 .UNSPECIFIED.,.F.,.F.,(4,4),(-0.618164468641375,-4.9439619065339E-17),
 .UNSPECIFIED.);
#266=B_SPLINE_CURVE_WITH_KNOTS('',3,(#10650,#10651,#10652,#10653),
 .UNSPECIFIED.,.F.,.F.,(4,4),(3.0964814046186E-16,0.618164468641375),
 .UNSPECIFIED.);
#267=B_SPLINE_CURVE_WITH_KNOTS('',3,(#10654,#10655,#10656,#10657),
 .UNSPECIFIED.,.F.,.F.,(4,4),(-0.618164468641375,-0.0007797326135453),
 .UNSPECIFIED.);
#268=B_SPLINE_CURVE_WITH_KNOTS('',3,(#10683,#10684,#10685,#10686,#10687),
 .UNSPECIFIED.,.F.,.F.,(4,1,4),(-10.419271481025,-4.62277271319024,-0.27539863731415),
 .UNSPECIFIED.);
#269=B_SPLINE_CURVE_WITH_KNOTS('',3,(#10688,#10689,#10690,#10691,#10692),
 .UNSPECIFIED.,.F.,.F.,(4,1,4),(0.27539863731415,4.62277271319024,10.419271481025),
 .UNSPECIFIED.);
#270=B_SPLINE_CURVE_WITH_KNOTS('',3,(#10713,#10714,#10715,#10716),
 .UNSPECIFIED.,.F.,.F.,(4,4),(0.00110654915602046,0.618489359031386),
 .UNSPECIFIED.);
#271=B_SPLINE_CURVE_WITH_KNOTS('',3,(#10717,#10718,#10719,#10720),
 .UNSPECIFIED.,.F.,.F.,(4,4),(-0.618489359031386,6.93889390390723E-18),
 .UNSPECIFIED.);
#272=B_SPLINE_CURVE_WITH_KNOTS('',3,(#10760,#10761,#10762,#10763,#10764,
#10765,#10766,#10767,#10768,#10769,#10770,#10771,#10772,#10773,#10774,#10775,
#10776,#10777,#10778,#10779,#10780,#10781,#10782,#10783),.UNSPECIFIED.,
 .F.,.F.,(4,2,2,2,2,2,2,2,2,2,2,4),(-0.337265338267783,-0.250544943628509,
-0.208272806508042,-0.186542211788094,-0.176382978682897,-0.170925844043069,
-0.16639450677335,-0.161077381235501,-0.15182241135393,-0.115009181549223,
-0.030206004227969,0.),.UNSPECIFIED.);
#273=B_SPLINE_CURVE_WITH_KNOTS('',3,(#10788,#10789,#10790,#10791,#10792,
#10793,#10794,#10795,#10796,#10797,#10798,#10799,#10800,#10801,#10802,#10803,
#10804,#10805,#10806,#10807),.UNSPECIFIED.,.F.,.F.,(4,2,2,2,2,2,2,2,2,4),
(-0.240982594686416,-0.16829976149504,-0.141836598208813,-0.129116059226128,
-0.121962912034391,-0.115857591426886,-0.108506552485159,-0.0948769875819265,
-0.0364654790774683,0.),.UNSPECIFIED.);
#274=B_SPLINE_CURVE_WITH_KNOTS('',3,(#10812,#10813,#10814,#10815,#10816,
#10817,#10818,#10819,#10820,#10821,#10822,#10823,#10824,#10825,#10826,#10827,
#10828,#10829,#10830,#10831),.UNSPECIFIED.,.F.,.F.,(4,2,2,2,2,2,2,2,2,4),
(-0.240981214998207,-0.168303541671295,-0.141841407502325,-0.129121097580905,
-0.121968013294536,-0.115862708924237,-0.108511643765797,-0.0948818976588229,
-0.0364681276985956,0.),.UNSPECIFIED.);
#275=B_SPLINE_CURVE_WITH_KNOTS('',3,(#10836,#10837,#10838,#10839,#10840,
#10841,#10842,#10843,#10844,#10845,#10846,#10847,#10848,#10849,#10850,#10851,
#10852,#10853,#10854,#10855,#10856,#10857,#10858,#10859),.UNSPECIFIED.,
 .F.,.F.,(4,2,2,2,2,2,2,2,2,2,2,4),(-0.337269388373684,-0.250545316912909,
-0.208282401844766,-0.186554569827561,-0.176396213396297,-0.17093921790305,
-0.16640782243471,-0.161090427650893,-0.151834477986603,-0.115010808423941,
-0.0302102096065556,0.),.UNSPECIFIED.);
#276=B_SPLINE_CURVE_WITH_KNOTS('',3,(#10882,#10883,#10884,#10885),
 .UNSPECIFIED.,.F.,.F.,(4,4),(1.0454440030657,2.52465537163019),
 .UNSPECIFIED.);
#277=B_SPLINE_CURVE_WITH_KNOTS('',3,(#10887,#10888,#10889,#10890,#10891,
#10892,#10893,#10894,#10895,#10896,#10897,#10898,#10899,#10900,#10901,#10902,
#10903,#10904,#10905,#10906,#10907,#10908,#10909,#10910,#10911,#10912,#10913,
#10914),.UNSPECIFIED.,.F.,.F.,(4,3,3,3,3,3,3,3,3,4),(-0.152193408756968,
-0.128427023368412,-0.115107736263918,-0.0911810900745799,-0.0780377802127556,
-0.0652031397886901,-0.0414031558437525,-0.0389949527774582,-0.0152076153333754,
0.),.UNSPECIFIED.);
#278=B_SPLINE_CURVE_WITH_KNOTS('',3,(#10916,#10917,#10918,#10919),
 .UNSPECIFIED.,.F.,.F.,(4,4),(-3.44967454744645,-1.05170160817356),
 .UNSPECIFIED.);
#279=B_SPLINE_CURVE_WITH_KNOTS('',3,(#10921,#10922,#10923,#10924,#10925,
#10926,#10927,#10928,#10929,#10930,#10931,#10932,#10933,#10934,#10935,#10936,
#10937,#10938,#10939,#10940,#10941,#10942,#10943,#10944,#10945,#10946,#10947,
#10948),.UNSPECIFIED.,.F.,.F.,(4,3,3,3,3,3,3,3,3,4),(-0.152278960443096,
-0.128503570101575,-0.115218572146868,-0.09145408274965,-0.0870214650669139,
-0.0781562978024333,-0.0542566895399357,-0.03908030849237,-0.0153296112319379,
0.),.UNSPECIFIED.);
#280=B_SPLINE_CURVE_WITH_KNOTS('',3,(#10949,#10950,#10951,#10952),
 .UNSPECIFIED.,.F.,.F.,(4,4),(2.75501813708031,3.4476340663212),
 .UNSPECIFIED.);
#281=B_SPLINE_CURVE_WITH_KNOTS('',3,(#10974,#10975,#10976,#10977),
 .UNSPECIFIED.,.F.,.F.,(4,4),(7.24810383506675,7.89761558728778),
 .UNSPECIFIED.);
#282=B_SPLINE_CURVE_WITH_KNOTS('',3,(#10979,#10980,#10981,#10982,#10983,
#10984,#10985,#10986,#10987,#10988,#10989,#10990,#10991,#10992,#10993,#10994,
#10995,#10996,#10997,#10998,#10999,#11000,#11001,#11002,#11003,#11004,#11005,
#11006),.UNSPECIFIED.,.F.,.F.,(4,3,3,3,3,3,3,3,3,4),(-0.152278869104567,
-0.128548794904564,-0.115192257893812,-0.0912773536606376,-0.0781090575823055,
-0.0652724057916263,-0.0414819581560496,-0.0390493575290778,-0.015259721743698,
0.),.UNSPECIFIED.);
#283=B_SPLINE_CURVE_WITH_KNOTS('',3,(#11008,#11009,#11010,#11011),
 .UNSPECIFIED.,.F.,.F.,(4,4),(-9.94532343034734,-7.24519303641511),
 .UNSPECIFIED.);
#284=B_SPLINE_CURVE_WITH_KNOTS('',3,(#11013,#11014,#11015,#11016,#11017,
#11018,#11019,#11020,#11021,#11022,#11023,#11024,#11025,#11026,#11027,#11028,
#11029,#11030,#11031,#11032,#11033,#11034,#11035,#11036,#11037,#11038,#11039,
#11040),.UNSPECIFIED.,.F.,.F.,(4,3,3,3,3,3,3,3,3,4),(-0.152181623618259,
-0.128410404494075,-0.115248188224843,-0.0914746846046984,-0.0869904866333268,
-0.0783028696190655,-0.0543945376065823,-0.0391651209697638,-0.0153884182770307,
0.),.UNSPECIFIED.);
#285=B_SPLINE_CURVE_WITH_KNOTS('',3,(#11041,#11042,#11043,#11044),
 .UNSPECIFIED.,.F.,.F.,(4,4),(8.21380824320284,9.95046871680089),
 .UNSPECIFIED.);
#286=B_SPLINE_CURVE_WITH_KNOTS('',3,(#11047,#11048,#11049,#11050),
 .UNSPECIFIED.,.F.,.F.,(4,4),(2.80491490332713,3.45442665446657),
 .UNSPECIFIED.);
#287=B_SPLINE_CURVE_WITH_KNOTS('',3,(#11054,#11055,#11056,#11057),
 .UNSPECIFIED.,.F.,.F.,(4,4),(0.752061768057538,2.48872224644044),
 .UNSPECIFIED.);
#288=B_SPLINE_CURVE_WITH_KNOTS('',3,(#11265,#11266,#11267,#11268,#11269,
#11270),.UNSPECIFIED.,.F.,.F.,(4,2,4),(-0.606700505977711,-0.303383635264422,
-0.000339350725729326),.UNSPECIFIED.);
#289=B_SPLINE_CURVE_WITH_KNOTS('',3,(#11271,#11272,#11273,#11274,#11275,
#11276,#11277,#11278,#11279,#11280,#11281,#11282,#11283,#11284,#11285,#11286,
#11287,#11288,#11289,#11290,#11291,#11292,#11293,#11294,#11295,#11296,#11297,
#11298),.UNSPECIFIED.,.F.,.F.,(4,3,3,3,3,3,3,3,3,4),(-0.152173579228948,
-0.128423230539522,-0.115115104157663,-0.0911927259648815,-0.0780672068328041,
-0.0652082609452843,-0.0414117413801899,-0.0390174000215468,-0.0152300060615686,
0.),.UNSPECIFIED.);
#290=B_SPLINE_CURVE_WITH_KNOTS('',3,(#11299,#11300,#11301,#11302,#11303,
#11304),.UNSPECIFIED.,.F.,.F.,(4,2,4),(-0.606471894652381,-0.303383500305553,
-0.00011071898471493),.UNSPECIFIED.);
#291=B_SPLINE_CURVE_WITH_KNOTS('',3,(#11308,#11309,#11310,#11311,#11312,
#11313),.UNSPECIFIED.,.F.,.F.,(4,2,4),(-0.606240625011114,-0.303433113375332,
-0.00010938105916114),.UNSPECIFIED.);
#292=B_SPLINE_CURVE_WITH_KNOTS('',3,(#11315,#11316,#11317,#11318,#11319,
#11320,#11321,#11322,#11323,#11324,#11325,#11326,#11327,#11328,#11329,#11330,
#11331,#11332,#11333,#11334,#11335,#11336,#11337,#11338,#11339,#11340,#11341,
#11342),.UNSPECIFIED.,.F.,.F.,(4,3,3,3,3,3,3,3,3,4),(-0.152281454644235,
-0.128508102092242,-0.115234945630277,-0.0914677943501604,-0.0870276017853555,
-0.0781846052914712,-0.0542821334115454,-0.0390966859411886,-0.0153419673568312,
0.),.UNSPECIFIED.);
#293=B_SPLINE_CURVE_WITH_KNOTS('',3,(#11344,#11345,#11346,#11347,#11348,
#11349),.UNSPECIFIED.,.F.,.F.,(4,2,4),(-0.606758573154242,-0.303433157101101,
-0.000627306481538803),.UNSPECIFIED.);
#294=B_SPLINE_CURVE_WITH_KNOTS('',3,(#11355,#11356,#11357,#11358,#11359,
#11360),.UNSPECIFIED.,.F.,.F.,(4,2,4),(-0.60617382748,-0.303436117212405,
-7.2700296824213E-5),.UNSPECIFIED.);
#295=B_SPLINE_CURVE_WITH_KNOTS('',3,(#11362,#11363,#11364,#11365,#11366,
#11367,#11368,#11369,#11370,#11371,#11372,#11373,#11374,#11375,#11376,#11377,
#11378,#11379,#11380,#11381,#11382,#11383,#11384,#11385,#11386,#11387,#11388,
#11389),.UNSPECIFIED.,.F.,.F.,(4,3,3,3,3,3,3,3,3,4),(-0.152282154327755,
-0.128558036203745,-0.115201429639692,-0.0912891813973639,-0.0781219052297615,
-0.065279687589213,-0.0414913146723999,-0.0390591331507366,-0.0152683745546824,
0.),.UNSPECIFIED.);
#296=B_SPLINE_CURVE_WITH_KNOTS('',3,(#11393,#11394,#11395,#11396,#11397,
#11398,#11399,#11400,#11401,#11402,#11403,#11404,#11405,#11406,#11407,#11408,
#11409,#11410,#11411,#11412,#11413,#11414,#11415,#11416,#11417,#11418,#11419,
#11420),.UNSPECIFIED.,.F.,.F.,(4,3,3,3,3,3,3,3,3,4),(-0.152283066055976,
-0.128508717930245,-0.115216472798554,-0.091451700383826,-0.087022506454752,
-0.0781485278686168,-0.0542483994686567,-0.0390758108455304,-0.0153274175274101,
0.),.UNSPECIFIED.);
#297=B_SPLINE_CURVE_WITH_KNOTS('',3,(#11422,#11423,#11424,#11425,#11426,
#11427),.UNSPECIFIED.,.F.,.F.,(4,2,4),(-0.606800264911061,-0.303436147592132,
-0.000699137727853738),.UNSPECIFIED.);
#298=B_SPLINE_CURVE_WITH_KNOTS('',3,(#11432,#11433,#11434,#11435,#11436,
#11437),.UNSPECIFIED.,.F.,.F.,(4,2,4),(-0.606915279655722,-0.30363236403835,
-0.000516487074480598),.UNSPECIFIED.);
#299=B_SPLINE_CURVE_WITH_KNOTS('',3,(#11441,#11442,#11443,#11444,#11445,
#11446,#11447,#11448,#11449,#11450,#11451,#11452,#11453,#11454,#11455,#11456,
#11457,#11458,#11459,#11460,#11461,#11462,#11463,#11464,#11465,#11466,#11467,
#11468),.UNSPECIFIED.,.F.,.F.,(4,3,3,3,3,3,3,3,3,4),(-0.152205325335401,
-0.128433618138404,-0.115304790388008,-0.091527299141506,-0.0870178586418932,
-0.0783866443643876,-0.0544751548276533,-0.0392137310602028,-0.0154203878854647,
0.),.UNSPECIFIED.);
#300=B_SPLINE_CURVE_WITH_KNOTS('',3,(#11470,#11471,#11472,#11473,#11474,
#11475),.UNSPECIFIED.,.F.,.F.,(4,2,4),(-0.606752424187958,-0.303632696349781,
-0.000353591088346872),.UNSPECIFIED.);
#301=B_SPLINE_CURVE_WITH_KNOTS('',3,(#11481,#11482,#11483,#11484),
 .UNSPECIFIED.,.F.,.F.,(4,4),(0.0116023361771303,0.618489359031386),
 .UNSPECIFIED.);
#302=B_SPLINE_CURVE_WITH_KNOTS('',3,(#11488,#11489,#11490,#11491),
 .UNSPECIFIED.,.F.,.F.,(4,4),(-0.618489359031386,-0.01160233617713),
 .UNSPECIFIED.);
#303=B_SPLINE_CURVE_WITH_KNOTS('',3,(#11494,#11495,#11496,#11497),
 .UNSPECIFIED.,.F.,.F.,(4,4),(7.01593971618694,9.71770560667459),
 .UNSPECIFIED.);
#304=B_SPLINE_CURVE_WITH_KNOTS('',3,(#11498,#11499,#11500,#11501),
 .UNSPECIFIED.,.F.,.F.,(4,4),(0.505945342046796,3.20718651982575),
 .UNSPECIFIED.);
#305=B_SPLINE_CURVE_WITH_KNOTS('',3,(#11504,#11505,#11506,#11507,#11508,
#11509,#11510),.UNSPECIFIED.,.F.,.F.,(4,3,4),(3.40717417387402,5.11170895874517,
6.80746068626633),.UNSPECIFIED.);
#306=B_SPLINE_CURVE_WITH_KNOTS('',3,(#11513,#11514,#11515,#11516),
 .UNSPECIFIED.,.F.,.F.,(4,4),(7.00766573366377,9.41198845520559),
 .UNSPECIFIED.);
#307=B_SPLINE_CURVE_WITH_KNOTS('',3,(#11520,#11521,#11522,#11523),
 .UNSPECIFIED.,.F.,.F.,(4,4),(9.61248784142317,10.2217363065808),
 .UNSPECIFIED.);
#308=B_SPLINE_CURVE_WITH_KNOTS('',3,(#11524,#11525,#11526,#11527,#11528,
#11529,#11530,#11531,#11532,#11533,#11534,#11535,#11536,#11537,#11538,#11539,
#11540,#11541,#11542,#11543,#11544,#11545,#11546,#11547,#11548,#11549,#11550,
#11551),.UNSPECIFIED.,.F.,.F.,(4,3,3,3,3,3,3,3,3,4),(0.,0.0238103109064959,
0.0390781362249314,0.0628635086275546,0.0641230352384255,0.0780643700703951,
0.101962174814111,0.113803522271848,0.137549611554782,0.149564734365165),
 .UNSPECIFIED.);
#309=B_SPLINE_CURVE_WITH_KNOTS('',3,(#11555,#11556,#11557,#11558,#11559,
#11560,#11561,#11562,#11563,#11564,#11565,#11566,#11567,#11568,#11569,#11570,
#11571,#11572,#11573,#11574,#11575,#11576,#11577,#11578,#11579,#11580,#11581,
#11582,#11583,#11584,#11585),.UNSPECIFIED.,.F.,.F.,(4,3,3,3,3,3,3,3,3,3,
4),(0.,0.0535521515156599,0.107729685495911,0.117233338918226,0.171447998942947,
0.1923696899792,0.234191611538245,0.288659693466396,0.341410301570312,0.395549383747909,
0.448696573746633),.UNSPECIFIED.);
#310=B_SPLINE_CURVE_WITH_KNOTS('',3,(#11587,#11588,#11589,#11590),
 .UNSPECIFIED.,.F.,.F.,(4,4),(0.0255858263485814,0.973760737485873),
 .UNSPECIFIED.);
#311=B_SPLINE_CURVE_WITH_KNOTS('',3,(#11592,#11593,#11594,#11595,#11596,
#11597,#11598,#11599,#11600,#11601,#11602,#11603,#11604,#11605,#11606,#11607,
#11608,#11609,#11610,#11611,#11612,#11613,#11614,#11615,#11616,#11617,#11618,
#11619,#11620,#11621,#11622),.UNSPECIFIED.,.F.,.F.,(4,3,3,3,3,3,3,3,3,3,
4),(0.,0.0535144560117858,0.107726856902975,0.117300577410231,0.171517675930231,
0.195438847090422,0.234297456941738,0.289665153342662,0.345032849743585,
0.40043206955427,0.455831289364955),.UNSPECIFIED.);
#312=B_SPLINE_CURVE_WITH_KNOTS('',3,(#11626,#11627,#11628,#11629,#11630,
#11631,#11632,#11633,#11634,#11635,#11636,#11637,#11638,#11639,#11640,#11641,
#11642,#11643,#11644,#11645,#11646,#11647,#11648,#11649,#11650,#11651,#11652,
#11653,#11654,#11655,#11656),.UNSPECIFIED.,.F.,.F.,(4,3,3,3,3,3,3,3,3,3,
4),(0.,0.053505543180391,0.107714168832353,0.117253997025819,0.171473395203321,
0.195418854185489,0.234223199196375,0.289607016015183,0.344990832833991,
0.400409777473312,0.455828722112633),.UNSPECIFIED.);
#313=B_SPLINE_CURVE_WITH_KNOTS('',3,(#11658,#11659,#11660,#11661),
 .UNSPECIFIED.,.F.,.F.,(4,4),(0.0262392625141271,0.974414173651419),
 .UNSPECIFIED.);
#314=B_SPLINE_CURVE_WITH_KNOTS('',3,(#11663,#11664,#11665,#11666,#11667,
#11668,#11669,#11670,#11671,#11672,#11673,#11674,#11675,#11676,#11677,#11678,
#11679,#11680,#11681,#11682,#11683,#11684,#11685,#11686,#11687,#11688,#11689,
#11690,#11691,#11692,#11693),.UNSPECIFIED.,.F.,.F.,(4,3,3,3,3,3,3,3,3,3,
4),(0.,0.0535648734523888,0.107747221190676,0.117299947751206,0.171510987106922,
0.192397607227928,0.234296687348373,0.288768001369001,0.341469499352622,
0.395597672314973,0.448700135162036),.UNSPECIFIED.);
#315=B_SPLINE_CURVE_WITH_KNOTS('',3,(#11696,#11697,#11698,#11699,#11700,
#11701,#11702,#11703,#11704,#11705,#11706,#11707,#11708,#11709,#11710,#11711,
#11712,#11713,#11714,#11715,#11716,#11717,#11718,#11719,#11720),
 .UNSPECIFIED.,.F.,.F.,(4,3,3,3,3,3,3,3,4),(0.,0.0238141989470671,0.0391004231578824,
0.0641320992313133,0.0780996136084711,0.101998806889826,0.113823260594808,
0.137564745199532,0.149565921982294),.UNSPECIFIED.);
#316=B_SPLINE_CURVE_WITH_KNOTS('',3,(#11722,#11723,#11724,#11725),
 .UNSPECIFIED.,.F.,.F.,(4,4),(2.76692059912875E-5,0.609394470571143),
 .UNSPECIFIED.);
#317=B_SPLINE_CURVE_WITH_KNOTS('',3,(#11728,#11729,#11730,#11731),
 .UNSPECIFIED.,.F.,.F.,(4,4),(0.809932799154201,3.21472245120952),
 .UNSPECIFIED.);
#318=B_SPLINE_CURVE_WITH_KNOTS('',3,(#11734,#11735,#11736,#11737,#11738,
#11739,#11740),.UNSPECIFIED.,.F.,.F.,(4,3,4),(3.41496637450242,5.11093193409745,
6.81591321610411),.UNSPECIFIED.);
#319=B_SPLINE_CURVE_WITH_KNOTS('',3,(#11744,#11745,#11746,#11747),
 .UNSPECIFIED.,.F.,.F.,(4,4),(9.91798263530139,10.2237206759544),
 .UNSPECIFIED.);
#320=B_SPLINE_CURVE_WITH_KNOTS('',3,(#11749,#11750,#11751,#11752,#11753,
#11754,#11755,#11756,#11757,#11758,#11759,#11760,#11761,#11762,#11763,#11764,
#11765,#11766,#11767,#11768,#11769,#11770,#11771,#11772,#11773,#11774,#11775,
#11776),.UNSPECIFIED.,.F.,.F.,(4,3,3,3,3,3,3,3,3,4),(0.,0.023807020713713,
0.039085080816122,0.0628703378723092,0.0651394887354207,0.0780750047750988,
0.101981498769656,0.114997221725907,0.138748569029605,0.151942344104828),
 .UNSPECIFIED.);
#321=B_SPLINE_CURVE_WITH_KNOTS('',3,(#11780,#11781,#11782,#11783,#11784,
#11785,#11786,#11787,#11788,#11789,#11790,#11791,#11792,#11793,#11794,#11795,
#11796,#11797,#11798,#11799,#11800,#11801,#11802,#11803,#11804,#11805,#11806,
#11807),.UNSPECIFIED.,.F.,.F.,(4,3,3,3,3,3,3,3,3,4),(0.,0.0238098191818892,
0.0391006681981376,0.0628849269680955,0.0651459659463291,0.0780999162396042,
0.102007524384594,0.115011225379555,0.138759376430353,0.151943200125079),
 .UNSPECIFIED.);
#322=B_SPLINE_CURVE_WITH_KNOTS('',3,(#11809,#11810,#11811,#11812),
 .UNSPECIFIED.,.F.,.F.,(4,4),(2.85486020485948E-5,0.305707210239178),
 .UNSPECIFIED.);
#323=B_SPLINE_CURVE_WITH_KNOTS('',3,(#11822,#11823,#11824,#11825,#11826,
#11827),.UNSPECIFIED.,.F.,.F.,(4,2,4),(-0.606446248197249,-0.303383959626182,
-6.4365448350312E-5),.UNSPECIFIED.);
#324=B_SPLINE_CURVE_WITH_KNOTS('',3,(#11829,#11830,#11831,#11832,#11833,
#11834),.UNSPECIFIED.,.F.,.F.,(4,2,4),(-0.60675170080159,-0.303384112192838,
-0.000369837888147484),.UNSPECIFIED.);
#325=B_SPLINE_CURVE_WITH_KNOTS('',3,(#11836,#11837,#11838,#11839,#11840,
#11841,#11842,#11843,#11844,#11845,#11846,#11847,#11848,#11849,#11850,#11851,
#11852,#11853,#11854,#11855,#11856,#11857,#11858,#11859,#11860,#11861,#11862,
#11863),.UNSPECIFIED.,.F.,.F.,(4,3,3,3,3,3,3,3,3,4),(-0.152162866344201,
-0.128411131698784,-0.115108013904405,-0.0911850729173883,-0.0780642464630149,
-0.0652023242402653,-0.0414053499882389,-0.0390151293250392,-0.0152279490549848,
0.),.UNSPECIFIED.);
#326=B_SPLINE_CURVE_WITH_KNOTS('',3,(#11866,#11867,#11868,#11869,#11870,
#11871,#11872,#11873,#11874,#11875,#11876,#11877,#11878,#11879,#11880,#11881,
#11882,#11883,#11884,#11885,#11886,#11887,#11888,#11889,#11890,#11891,#11892,
#11893),.UNSPECIFIED.,.F.,.F.,(4,3,3,3,3,3,3,3,3,4),(-0.152171297476962,
-0.128400300768352,-0.115247520946962,-0.0914735511738372,-0.0869860114952295,
-0.0783112904282795,-0.0544025203706761,-0.0391699941254272,-0.015391764586027,
0.),.UNSPECIFIED.);
#327=B_SPLINE_CURVE_WITH_KNOTS('',3,(#11910,#11911,#11912,#11913),
 .UNSPECIFIED.,.F.,.F.,(4,4),(-3.45733745322815,-0.757207059295936),
 .UNSPECIFIED.);
#328=B_SPLINE_CURVE_WITH_KNOTS('',3,(#11931,#11932,#11933,#11934),
 .UNSPECIFIED.,.F.,.F.,(4,4),(-0.557056952888827,-0.283259008618247),
 .UNSPECIFIED.);
#329=B_SPLINE_CURVE_WITH_KNOTS('',3,(#11935,#11936,#11937,#11938),
 .UNSPECIFIED.,.F.,.F.,(4,4),(-0.618164468641375,-0.0110156167597059),
 .UNSPECIFIED.);
#330=B_SPLINE_CURVE_WITH_KNOTS('',3,(#11980,#11981,#11982,#11983),
 .UNSPECIFIED.,.F.,.F.,(4,4),(0.283259011433088,0.551788488929761),
 .UNSPECIFIED.);
#331=B_SPLINE_CURVE_WITH_KNOTS('',3,(#11987,#11988,#11989,#11990),
 .UNSPECIFIED.,.F.,.F.,(4,4),(10.1507419987596,10.419271481025),
 .UNSPECIFIED.);
#332=B_SPLINE_CURVE_WITH_KNOTS('',3,(#12025,#12026,#12027,#12028),
 .UNSPECIFIED.,.F.,.F.,(4,4),(0.0110156167597055,0.618164468641375),
 .UNSPECIFIED.);
#333=B_SPLINE_CURVE_WITH_KNOTS('',3,(#12029,#12030,#12031,#12032),
 .UNSPECIFIED.,.F.,.F.,(4,4),(-10.419271481025,-10.1454735367545),
 .UNSPECIFIED.);
#334=B_SPLINE_CURVE_WITH_KNOTS('',3,(#12035,#12036,#12037,#12038,#12039,
#12040),.UNSPECIFIED.,.F.,.F.,(4,2,4),(-0.606211482799139,-0.303431960476852,
-9.19895310989571E-5),.UNSPECIFIED.);
#335=B_SPLINE_CURVE_WITH_KNOTS('',3,(#12042,#12043,#12044,#12045,#12046,
#12047,#12048,#12049,#12050,#12051,#12052,#12053,#12054,#12055,#12056,#12057,
#12058,#12059,#12060,#12061,#12062,#12063,#12064,#12065,#12066,#12067,#12068,
#12069),.UNSPECIFIED.,.F.,.F.,(4,3,3,3,3,3,3,3,3,4),(-0.152283340966725,
-0.128554242174982,-0.115196092098682,-0.0912819860997417,-0.0781117853096875,
-0.0652755629514801,-0.0414857317972147,-0.039051434275634,-0.0152612146291672,
0.),.UNSPECIFIED.);
#336=B_SPLINE_CURVE_WITH_KNOTS('',3,(#12073,#12074,#12075,#12076,#12077,
#12078,#12079,#12080,#12081,#12082,#12083,#12084,#12085,#12086,#12087,#12088,
#12089,#12090,#12091,#12092,#12093,#12094,#12095,#12096,#12097,#12098,#12099,
#12100),.UNSPECIFIED.,.F.,.F.,(4,3,3,3,3,3,3,3,3,4),(-0.152285570909379,
-0.128511627155755,-0.115232904621082,-0.0914664612111958,-0.0870286654075453,
-0.0781769338106538,-0.0542752301960614,-0.039092246575741,-0.0153386136911565,
0.),.UNSPECIFIED.);
#337=B_SPLINE_CURVE_WITH_KNOTS('',3,(#12101,#12102,#12103,#12104,#12105,
#12106),.UNSPECIFIED.,.F.,.F.,(4,2,4),(-0.606773318344362,-0.303431998667662,
-0.000653802131222458),.UNSPECIFIED.);
#338=B_SPLINE_CURVE_WITH_KNOTS('',3,(#12123,#12124,#12125,#12126),
 .UNSPECIFIED.,.F.,.F.,(4,4),(-7.05313168653828,-3.6572084986735),
 .UNSPECIFIED.);
#339=B_SPLINE_CURVE_WITH_KNOTS('',3,(#12147,#12148,#12149,#12150),
 .UNSPECIFIED.,.F.,.F.,(4,4),(3.65450559744172,7.0548588409572),
 .UNSPECIFIED.);
#340=B_SPLINE_CURVE_WITH_KNOTS('',3,(#12152,#12153,#12154,#12155),
 .UNSPECIFIED.,.F.,.F.,(4,4),(3.64767164868607,7.04802489220155),
 .UNSPECIFIED.);
#341=B_SPLINE_CURVE_WITH_KNOTS('',3,(#12176,#12177,#12178,#12179),
 .UNSPECIFIED.,.F.,.F.,(4,4),(-7.04532199096977,-3.64939880310499),
 .UNSPECIFIED.);
#342=B_SPLINE_CURVE_WITH_KNOTS('',3,(#12198,#12199,#12200,#12201,#12202,
#12203),.UNSPECIFIED.,.F.,.F.,(4,2,4),(-0.606200453641641,-0.30343602424441,
-9.0120313562092E-5),.UNSPECIFIED.);
#343=B_SPLINE_CURVE_WITH_KNOTS('',3,(#12205,#12206,#12207,#12208,#12209,
#12210,#12211,#12212,#12213,#12214,#12215,#12216,#12217,#12218,#12219,#12220,
#12221,#12222,#12223,#12224,#12225,#12226,#12227,#12228,#12229,#12230,#12231,
#12232),.UNSPECIFIED.,.F.,.F.,(4,3,3,3,3,3,3,3,3,4),(-0.152277688086818,
-0.128551334178815,-0.115197577176818,-0.0912856014461669,-0.0781191417238373,
-0.0652765169533013,-0.0414883027365163,-0.0390570310290822,-0.0152653090895913,
0.),.UNSPECIFIED.);
#344=B_SPLINE_CURVE_WITH_KNOTS('',3,(#12234,#12235,#12236,#12237,#12238,
#12239),.UNSPECIFIED.,.F.,.F.,(4,2,4),(-0.60678286609787,-0.303436074842897,
-0.000672492961417026),.UNSPECIFIED.);
#345=B_SPLINE_CURVE_WITH_KNOTS('',3,(#12256,#12257,#12258,#12259),
 .UNSPECIFIED.,.F.,.F.,(4,4),(-9.65082888146972,-7.25285594219682),
 .UNSPECIFIED.);
#346=B_SPLINE_CURVE_WITH_KNOTS('',3,(#12280,#12281,#12282,#12283),
 .UNSPECIFIED.,.F.,.F.,(4,4),(7.25489642332205,7.94751235889625),
 .UNSPECIFIED.);
#347=B_SPLINE_CURVE_WITH_KNOTS('',3,(#12284,#12285,#12286,#12287),
 .UNSPECIFIED.,.F.,.F.,(4,4),(8.17787511801303,9.65708648657758),
 .UNSPECIFIED.);
#348=B_SPLINE_CURVE_WITH_KNOTS('',3,(#12307,#12308,#12309,#12310,#12311,
#12312),.UNSPECIFIED.,.F.,.F.,(4,2,4),(-0.607007797795788,-0.303636495504298,
-0.000571323176327465),.UNSPECIFIED.);
#349=B_SPLINE_CURVE_WITH_KNOTS('',3,(#12314,#12315,#12316,#12317,#12318,
#12319,#12320,#12321,#12322,#12323,#12324,#12325,#12326,#12327,#12328,#12329,
#12330,#12331,#12332,#12333,#12334,#12335,#12336,#12337,#12338,#12339,#12340,
#12341),.UNSPECIFIED.,.F.,.F.,(4,3,3,3,3,3,3,3,3,4),(-0.152184339020145,
-0.128410461444444,-0.115096394428865,-0.0911692948751363,-0.0780261759644403,
-0.0651939085034322,-0.0413932235702045,-0.0389860720679279,-0.0151971168406065,
0.),.UNSPECIFIED.);
#350=B_SPLINE_CURVE_WITH_KNOTS('',3,(#12345,#12346,#12347,#12348,#12349,
#12350,#12351,#12352,#12353,#12354,#12355,#12356,#12357,#12358,#12359,#12360,
#12361,#12362,#12363,#12364,#12365,#12366,#12367,#12368,#12369,#12370,#12371,
#12372),.UNSPECIFIED.,.F.,.F.,(4,3,3,3,3,3,3,3,3,4),(-0.15219777746951,
-0.128424216118147,-0.115318679085322,-0.0915406112613293,-0.0870190514838729,
-0.0784197287877601,-0.0545085386658457,-0.0392329067084975,-0.0154317870320417,
0.),.UNSPECIFIED.);
#351=B_SPLINE_CURVE_WITH_KNOTS('',3,(#12373,#12374,#12375,#12376,#12377,
#12378),.UNSPECIFIED.,.F.,.F.,(4,2,4),(-0.606706256981509,-0.303636876939173,
-0.00026974181288697),.UNSPECIFIED.);
#352=B_SPLINE_CURVE_WITH_KNOTS('',3,(#12396,#12397,#12398,#12399),
 .UNSPECIFIED.,.F.,.F.,(4,4),(0.0112334529114386,0.618489359031386),
 .UNSPECIFIED.);
#353=B_SPLINE_CURVE_WITH_KNOTS('',3,(#12400,#12401,#12402,#12403),
 .UNSPECIFIED.,.F.,.F.,(4,4),(-10.4271318523291,-9.85085636625011),
 .UNSPECIFIED.);
#354=B_SPLINE_CURVE_WITH_KNOTS('',3,(#12426,#12427,#12428,#12429),
 .UNSPECIFIED.,.F.,.F.,(4,4),(9.85750350611301,10.4271318523291),
 .UNSPECIFIED.);
#355=B_SPLINE_CURVE_WITH_KNOTS('',3,(#12433,#12434,#12435,#12436),
 .UNSPECIFIED.,.F.,.F.,(4,4),(0.27539863731415,0.845026983530265),
 .UNSPECIFIED.);
#356=B_SPLINE_CURVE_WITH_KNOTS('',3,(#12454,#12455,#12456,#12457),
 .UNSPECIFIED.,.F.,.F.,(4,4),(-0.851674123393175,-0.27539863731415),
 .UNSPECIFIED.);
#357=B_SPLINE_CURVE_WITH_KNOTS('',3,(#12458,#12459,#12460,#12461),
 .UNSPECIFIED.,.F.,.F.,(4,4),(-0.618489359031386,-0.0112334529114389),
 .UNSPECIFIED.);
#358=B_SPLINE_CURVE_WITH_KNOTS('',3,(#12541,#12542,#12543,#12544),
 .UNSPECIFIED.,.F.,.F.,(4,4),(0.0112755522169305,0.618164468641375),
 .UNSPECIFIED.);
#359=B_SPLINE_CURVE_WITH_KNOTS('',3,(#12565,#12566,#12567,#12568),
 .UNSPECIFIED.,.F.,.F.,(4,4),(-0.618164468641375,-0.0112755522169305),
 .UNSPECIFIED.);
#360=B_SPLINE_CURVE_WITH_KNOTS('',3,(#12654,#12655,#12656,#12657),
 .UNSPECIFIED.,.F.,.F.,(4,4),(5.55111512312578E-17,0.618489359031386),
 .UNSPECIFIED.);
#361=B_SPLINE_CURVE_WITH_KNOTS('',3,(#12658,#12659,#12660,#12661),
 .UNSPECIFIED.,.F.,.F.,(4,4),(-0.618489359031386,-0.00110654915602034),
 .UNSPECIFIED.);
#362=B_SPLINE_CURVE_WITH_KNOTS('',3,(#12697,#12698,#12699,#12700,#12701),
 .UNSPECIFIED.,.F.,.F.,(4,1,4),(-10.4271318523291,-4.63063308449434,-0.283259008618247),
 .UNSPECIFIED.);
#363=B_SPLINE_CURVE_WITH_KNOTS('',3,(#12702,#12703,#12704,#12705,#12706),
 .UNSPECIFIED.,.F.,.F.,(4,1,4),(0.283259011433087,4.63063308449434,10.4271318523291),
 .UNSPECIFIED.);
#364=B_SPLINE_CURVE_WITH_KNOTS('',3,(#12727,#12728,#12729,#12730),
 .UNSPECIFIED.,.F.,.F.,(4,4),(0.000779732613545348,0.618164468641375),
 .UNSPECIFIED.);
#365=B_SPLINE_CURVE_WITH_KNOTS('',3,(#12731,#12732,#12733,#12734),
 .UNSPECIFIED.,.F.,.F.,(4,4),(-0.618164468641375,-4.9439619065339E-17),
 .UNSPECIFIED.);
#366=B_SPLINE_CURVE_WITH_KNOTS('',3,(#12755,#12756,#12757,#12758),
 .UNSPECIFIED.,.F.,.F.,(4,4),(3.0964814046186E-16,0.618164468641375),
 .UNSPECIFIED.);
#367=B_SPLINE_CURVE_WITH_KNOTS('',3,(#12759,#12760,#12761,#12762),
 .UNSPECIFIED.,.F.,.F.,(4,4),(-0.618164468641375,-0.0007797326135453),
 .UNSPECIFIED.);
#368=B_SPLINE_CURVE_WITH_KNOTS('',3,(#12788,#12789,#12790,#12791,#12792),
 .UNSPECIFIED.,.F.,.F.,(4,1,4),(-10.419271481025,-4.62277271319024,-0.27539863731415),
 .UNSPECIFIED.);
#369=B_SPLINE_CURVE_WITH_KNOTS('',3,(#12793,#12794,#12795,#12796,#12797),
 .UNSPECIFIED.,.F.,.F.,(4,1,4),(0.27539863731415,4.62277271319024,10.419271481025),
 .UNSPECIFIED.);
#370=B_SPLINE_CURVE_WITH_KNOTS('',3,(#12818,#12819,#12820,#12821),
 .UNSPECIFIED.,.F.,.F.,(4,4),(0.00110654915602046,0.618489359031386),
 .UNSPECIFIED.);
#371=B_SPLINE_CURVE_WITH_KNOTS('',3,(#12822,#12823,#12824,#12825),
 .UNSPECIFIED.,.F.,.F.,(4,4),(-0.618489359031386,6.93889390390723E-18),
 .UNSPECIFIED.);
#372=B_SPLINE_CURVE_WITH_KNOTS('',3,(#12867,#12868,#12869,#12870,#12871,
#12872,#12873,#12874,#12875,#12876),.UNSPECIFIED.,.F.,.F.,(4,3,3,4),(-4.09202352044852,
-3.99057144343763,-2.99292858257822,-2.07317267331971),.UNSPECIFIED.);
#373=B_SPLINE_CURVE_WITH_KNOTS('',3,(#12879,#12880,#12881,#12882,#12883,
#12884,#12885),.UNSPECIFIED.,.F.,.F.,(4,3,4),(0.,0.998042281124014,1.12274180646116),
 .UNSPECIFIED.);
#374=B_SPLINE_CURVE_WITH_KNOTS('',3,(#12890,#12891,#12892,#12893,#12894,
#12895,#12896,#12897,#12898,#12899,#12900,#12901,#12902,#12903,#12904,#12905,
#12906,#12907,#12908,#12909,#12910,#12911),.UNSPECIFIED.,.F.,.F.,(4,3,3,
3,3,3,3,4),(-10.3752088276281,-9.97642860859406,-8.97878574773466,-7.98114288687525,
-6.98350002601584,-5.98585716515644,-4.98821430429703,-4.09202352044852),
 .UNSPECIFIED.);
#375=B_SPLINE_CURVE_WITH_KNOTS('',3,(#12912,#12913,#12914,#12915,#12916,
#12917,#12918,#12919,#12920,#12921,#12922,#12923,#12924,#12925,#12926,#12927,
#12928,#12929,#12930,#12931,#12932,#12933),.UNSPECIFIED.,.F.,.F.,(4,3,3,
3,3,3,3,4),(1.12274180646116,1.99608456224804,2.99412684337208,3.99216912449611,
4.99021140562014,5.98825368674417,6.98629596786821,7.40592711364074),
 .UNSPECIFIED.);
#376=B_SPLINE_CURVE_WITH_KNOTS('',3,(#12938,#12939,#12940,#12941,#12942,
#12943,#12944,#12945,#12946,#12947,#12948,#12949,#12950,#12951,#12952,#12953,
#12954,#12955,#12956,#12957,#12958,#12959),.UNSPECIFIED.,.F.,.F.,(4,3,3,
3,3,3,3,4),(-16.6583941348077,-15.9622857737505,-14.9646429128911,-13.9670000520317,
-12.9693571911723,-11.9717143303129,-10.9740714694535,-10.3752088276281),
 .UNSPECIFIED.);
#377=B_SPLINE_CURVE_WITH_KNOTS('',3,(#12960,#12961,#12962,#12963,#12964,
#12965,#12966,#12967,#12968,#12969,#12970,#12971,#12972,#12973,#12974,#12975,
#12976,#12977,#12978,#12979,#12980,#12981),.UNSPECIFIED.,.F.,.F.,(4,3,3,
3,3,3,3,4),(7.40592711364074,7.98433824899223,8.98238053011626,9.98042281124028,
10.9784650923643,11.9765073734883,12.9745496546124,13.6891124208203),
 .UNSPECIFIED.);
#378=B_SPLINE_CURVE_WITH_KNOTS('',3,(#12986,#12987,#12988,#12989,#12990,
#12991,#12992,#12993,#12994,#12995,#12996,#12997,#12998,#12999,#13000,#13001,
#13002,#13003,#13004,#13005,#13006,#13007),.UNSPECIFIED.,.F.,.F.,(4,3,3,
3,3,3,3,4),(-22.9415794419873,-21.9481429389069,-20.9505000780475,-19.9528572171881,
-18.9552143563287,-17.9575714954693,-16.9599286346099,-16.6583941348077),
 .UNSPECIFIED.);
#379=B_SPLINE_CURVE_WITH_KNOTS('',3,(#13008,#13009,#13010,#13011,#13012,
#13013,#13014,#13015,#13016,#13017,#13018,#13019,#13020,#13021,#13022,#13023,
#13024,#13025,#13026,#13027,#13028,#13029,#13030,#13031,#13032),
 .UNSPECIFIED.,.F.,.F.,(4,3,3,3,3,3,3,3,4),(13.6891124208203,13.9725919357364,
14.9706342168604,15.9686764979844,16.9667187791085,17.9647610602325,18.9628033413565,
19.9608456224805,19.9722977279999),.UNSPECIFIED.);
#380=B_SPLINE_CURVE_WITH_KNOTS('',3,(#13037,#13038,#13039,#13040,#13041,
#13042,#13043,#13044,#13045,#13046,#13047,#13048,#13049,#13050,#13051,#13052,
#13053,#13054,#13055,#13056,#13057,#13058),.UNSPECIFIED.,.F.,.F.,(4,3,3,
3,3,3,3,4),(-29.2247647491669,-28.9316429649228,-27.9340001040634,-26.936357243204,
-25.9387143823446,-24.9410715214852,-23.9434286606257,-22.9415794419873),
 .UNSPECIFIED.);
#381=B_SPLINE_CURVE_WITH_KNOTS('',3,(#13059,#13060,#13061,#13062,#13063,
#13064,#13065,#13066,#13067,#13068,#13069,#13070,#13071,#13072,#13073,#13074,
#13075,#13076,#13077,#13078,#13079,#13080),.UNSPECIFIED.,.F.,.F.,(4,3,3,
3,3,3,3,4),(19.9722977279999,20.9588879036046,21.9569301847286,22.9549724658526,
23.9530147469767,24.9510570281007,25.9490993092247,26.2554830351795),
 .UNSPECIFIED.);
#382=B_SPLINE_CURVE_WITH_KNOTS('',3,(#13085,#13086,#13087,#13088,#13089,
#13090,#13091,#13092,#13093,#13094,#13095,#13096,#13097,#13098,#13099,#13100,
#13101,#13102,#13103,#13104,#13105,#13106),.UNSPECIFIED.,.F.,.F.,(4,3,3,
3,3,3,3,4),(-35.5079500563465,-34.9175001300792,-33.9198572692198,-32.9222144083604,
-31.924571547501,-30.9269286866416,-29.9292858257822,-29.2247647491669),
 .UNSPECIFIED.);
#383=B_SPLINE_CURVE_WITH_KNOTS('',3,(#13107,#13108,#13109,#13110,#13111,
#13112,#13113,#13114,#13115,#13116,#13117,#13118,#13119,#13120,#13121,#13122,
#13123,#13124,#13125,#13126,#13127,#13128),.UNSPECIFIED.,.F.,.F.,(4,3,3,
3,3,3,3,4),(26.2554830351795,26.9471415903487,27.9451838714728,28.9432261525968,
29.9412684337208,30.9393107148448,31.9373529959689,32.5386683423591),
 .UNSPECIFIED.);
#384=B_SPLINE_CURVE_WITH_KNOTS('',3,(#13133,#13134,#13135,#13136,#13137,
#13138,#13139,#13140,#13141,#13142,#13143,#13144,#13145,#13146,#13147,#13148,
#13149,#13150,#13151,#13152,#13153,#13154),.UNSPECIFIED.,.F.,.F.,(4,3,3,
3,3,3,3,4),(-41.791135363526,-40.9033572952357,-39.9057144343762,-38.9080715735168,
-37.9104287126574,-36.912785851798,-35.9151429909386,-35.5079500563465),
 .UNSPECIFIED.);
#385=B_SPLINE_CURVE_WITH_KNOTS('',3,(#13155,#13156,#13157,#13158,#13159,
#13160,#13161,#13162,#13163,#13164,#13165,#13166,#13167,#13168,#13169,#13170,
#13171,#13172,#13173,#13174,#13175,#13176),.UNSPECIFIED.,.F.,.F.,(4,3,3,
3,3,3,3,4),(32.5386683423591,32.9353952770929,33.9334375582169,34.931479839341,
35.929522120465,36.927564401589,37.9256066827131,38.8218536495387),
 .UNSPECIFIED.);
#386=B_SPLINE_CURVE_WITH_KNOTS('',3,(#13181,#13182,#13183,#13184,#13185,
#13186,#13187,#13188,#13189,#13190,#13191,#13192,#13193,#13194,#13195,#13196,
#13197,#13198,#13199,#13200,#13201,#13202,#13203,#13204,#13205),
 .UNSPECIFIED.,.F.,.F.,(4,3,3,3,3,3,3,3,4),(-48.0743206707056,-47.8868573212515,
-46.8892144603921,-45.8915715995327,-44.8939287386733,-43.8962858778139,
-42.8986430169545,-41.9010001560951,-41.791135363526),.UNSPECIFIED.);
#387=B_SPLINE_CURVE_WITH_KNOTS('',3,(#13206,#13207,#13208,#13209,#13210,
#13211,#13212,#13213,#13214,#13215,#13216,#13217,#13218,#13219,#13220,#13221,
#13222,#13223,#13224,#13225,#13226,#13227,#13228,#13229,#13230),
 .UNSPECIFIED.,.F.,.F.,(4,3,3,3,3,3,3,3,4),(38.8218536495387,38.9236489638371,
39.9216912449611,40.9197335260851,41.9177758072091,42.9158180883332,43.9138603694572,
44.9119026505812,45.1050389567183),.UNSPECIFIED.);
#388=B_SPLINE_CURVE_WITH_KNOTS('',3,(#13235,#13236,#13237,#13238,#13239,
#13240,#13241,#13242,#13243,#13244,#13245,#13246,#13247,#13248,#13249,#13250,
#13251,#13252,#13253,#13254,#13255,#13256),.UNSPECIFIED.,.F.,.F.,(4,3,3,
3,3,3,3,4),(-54.3575059778852,-53.8727144864079,-52.8750716255485,-51.8774287646891,
-50.8797859038297,-49.8821430429703,-48.8845001821109,-48.0743206707056),
 .UNSPECIFIED.);
#389=B_SPLINE_CURVE_WITH_KNOTS('',3,(#13257,#13258,#13259,#13260,#13261,
#13262,#13263,#13264,#13265,#13266,#13267,#13268,#13269,#13270,#13271,#13272,
#13273,#13274,#13275,#13276,#13277,#13278),.UNSPECIFIED.,.F.,.F.,(4,3,3,
3,3,3,3,4),(45.1050389567183,45.9099449317052,46.9079872128293,47.9060294939533,
48.9040717750773,49.9021140562014,50.9001563373254,51.3882242638979),
 .UNSPECIFIED.);
#390=B_SPLINE_CURVE_WITH_KNOTS('',3,(#13283,#13284,#13285,#13286,#13287,
#13288,#13289,#13290,#13291,#13292,#13293,#13294,#13295,#13296,#13297,#13298,
#13299,#13300,#13301,#13302,#13303,#13304),.UNSPECIFIED.,.F.,.F.,(4,3,3,
3,3,3,3,4),(-60.6406912850648,-59.8585716515644,-58.860928790705,-57.8632859298455,
-56.8656430689861,-55.8680002081267,-54.8703573472673,-54.3575059778852),
 .UNSPECIFIED.);
#391=B_SPLINE_CURVE_WITH_KNOTS('',3,(#13305,#13306,#13307,#13308,#13309,
#13310,#13311,#13312,#13313,#13314,#13315,#13316,#13317,#13318,#13319,#13320,
#13321,#13322,#13323,#13324,#13325,#13326),.UNSPECIFIED.,.F.,.F.,(4,3,3,
3,3,3,3,4),(51.3882242638979,51.8981986184494,52.8962408995734,53.8942831806975,
54.8923254618215,55.8903677429455,56.8884100240695,57.6714095710775),
 .UNSPECIFIED.);
#392=B_SPLINE_CURVE_WITH_KNOTS('',3,(#13331,#13332,#13333,#13334,#13335,
#13336,#13337,#13338,#13339,#13340,#13341,#13342,#13343,#13344,#13345,#13346,
#13347,#13348,#13349,#13350,#13351,#13352,#13353,#13354,#13355),
 .UNSPECIFIED.,.F.,.F.,(4,3,3,3,3,3,3,3,4),(-66.9238765922444,-66.8420716775802,
-65.8444288167208,-64.8467859558614,-63.849143095002,-62.8515002341426,
-61.8538573732832,-60.8562145124238,-60.6406912850648),.UNSPECIFIED.);
#393=B_SPLINE_CURVE_WITH_KNOTS('',3,(#13356,#13357,#13358,#13359,#13360,
#13361,#13362,#13363,#13364,#13365,#13366,#13367,#13368,#13369,#13370,#13371,
#13372,#13373,#13374,#13375,#13376,#13377,#13378,#13379,#13380),
 .UNSPECIFIED.,.F.,.F.,(4,3,3,3,3,3,3,3,4),(57.6714095710775,57.8864523051936,
58.8844945863176,59.8825368674416,60.8805791485657,61.8786214296897,62.8766637108137,
63.8747059919378,63.9545948782571),.UNSPECIFIED.);
#394=B_SPLINE_CURVE_WITH_KNOTS('',3,(#13385,#13386,#13387,#13388,#13389,
#13390,#13391,#13392,#13393,#13394,#13395,#13396,#13397,#13398,#13399,#13400,
#13401,#13402,#13403,#13404,#13405,#13406),.UNSPECIFIED.,.F.,.F.,(4,3,3,
3,3,3,3,4),(-73.207061899424,-72.8279288427366,-71.8302859818773,-70.8326431210178,
-69.8350002601584,-68.837357399299,-67.8397145384396,-66.9238765922444),
 .UNSPECIFIED.);
#395=B_SPLINE_CURVE_WITH_KNOTS('',3,(#13407,#13408,#13409,#13410,#13411,
#13412,#13413,#13414,#13415,#13416,#13417,#13418,#13419,#13420,#13421,#13422,
#13423,#13424,#13425,#13426,#13427,#13428),.UNSPECIFIED.,.F.,.F.,(4,3,3,
3,3,3,3,4),(63.9545948782571,64.8727482730618,65.8707905541858,66.8688328353098,
67.8668751164338,68.8649173975579,69.8629596786819,70.2377801854366),
 .UNSPECIFIED.);
#396=B_SPLINE_CURVE_WITH_KNOTS('',3,(#13433,#13434,#13435,#13436,#13437,
#13438,#13439,#13440,#13441,#13442,#13443,#13444,#13445,#13446,#13447,#13448,
#13449,#13450,#13451,#13452,#13453,#13454),.UNSPECIFIED.,.F.,.F.,(4,3,3,
3,3,3,3,4),(-79.4902472066036,-78.8137860078931,-77.8161431470337,-76.8185002861743,
-75.8208574253149,-74.8232145644555,-73.825571703596,-73.207061899424),
 .UNSPECIFIED.);
#397=B_SPLINE_CURVE_WITH_KNOTS('',3,(#13455,#13456,#13457,#13458,#13459,
#13460,#13461,#13462,#13463,#13464,#13465,#13466,#13467,#13468,#13469,#13470,
#13471,#13472,#13473,#13474,#13475,#13476),.UNSPECIFIED.,.F.,.F.,(4,3,3,
3,3,3,3,4),(70.2377801854366,70.8610019598059,71.85904424093,72.857086522054,
73.855128803178,74.853171084302,75.8512133654261,76.5209654926162),
 .UNSPECIFIED.);
#398=B_SPLINE_CURVE_WITH_KNOTS('',3,(#13481,#13482,#13483,#13484,#13485,
#13486,#13487,#13488,#13489,#13490,#13491,#13492,#13493,#13494,#13495,#13496,
#13497,#13498,#13499,#13500,#13501,#13502),.UNSPECIFIED.,.F.,.F.,(4,3,3,
3,3,3,3,4),(-85.7734325137832,-84.7996431730495,-83.8020003121901,-82.8043574513307,
-81.8067145904713,-80.8090717296119,-79.8114288687525,-79.4902472066036),
 .UNSPECIFIED.);
#399=B_SPLINE_CURVE_WITH_KNOTS('',3,(#13503,#13504,#13505,#13506,#13507,
#13508,#13509,#13510,#13511,#13512,#13513,#13514,#13515,#13516,#13517,#13518,
#13519,#13520,#13521,#13522,#13523,#13524),.UNSPECIFIED.,.F.,.F.,(4,3,3,
3,3,3,3,4),(76.5209654926162,76.8492556465501,77.8472979276741,78.8453402087982,
79.8433824899222,80.8414247710462,81.8394670521702,82.8041507997958),
 .UNSPECIFIED.);
#400=B_SPLINE_CURVE_WITH_KNOTS('',3,(#13529,#13530,#13531,#13532,#13533,
#13534,#13535,#13536,#13537,#13538,#13539,#13540,#13541,#13542,#13543,#13544,
#13545,#13546,#13547,#13548,#13549,#13550,#13551,#13552,#13553),
 .UNSPECIFIED.,.F.,.F.,(4,3,3,3,3,3,3,3,4),(-92.0566178209628,-91.7831431990654,
-90.7855003382059,-89.7878574773465,-88.7902146164871,-87.7925717556277,
-86.7949288947683,-85.7972860339089,-85.7734325137832),.UNSPECIFIED.);
#401=B_SPLINE_CURVE_WITH_KNOTS('',3,(#13554,#13555,#13556,#13557,#13558,
#13559,#13560,#13561,#13562,#13563,#13564,#13565,#13566,#13567,#13568,#13569,
#13570,#13571,#13572,#13573,#13574,#13575,#13576,#13577,#13578),
 .UNSPECIFIED.,.F.,.F.,(4,3,3,3,3,3,3,3,4),(82.8041507997958,82.8375093332942,
83.8355516144183,84.8335938955423,85.8316361766664,86.8296784577904,87.8277207389144,
88.8257630200384,89.0873361069754),.UNSPECIFIED.);
#402=B_SPLINE_CURVE_WITH_KNOTS('',3,(#13583,#13584,#13585,#13586,#13587,
#13588,#13589,#13590,#13591,#13592,#13593,#13594,#13595,#13596,#13597,#13598,
#13599,#13600,#13601,#13602,#13603,#13604),.UNSPECIFIED.,.F.,.F.,(4,3,3,
3,3,3,3,4),(-98.3398031281424,-97.7690003642218,-96.7713575033624,-95.773714642503,
-94.7760717816436,-93.7784289207842,-92.7807860599248,-92.0566178209628),
 .UNSPECIFIED.);
#403=B_SPLINE_CURVE_WITH_KNOTS('',3,(#13605,#13606,#13607,#13608,#13609,
#13610,#13611,#13612,#13613,#13614,#13615,#13616,#13617,#13618,#13619,#13620,
#13621,#13622,#13623,#13624,#13625,#13626),.UNSPECIFIED.,.F.,.F.,(4,3,3,
3,3,3,3,4),(89.0873361069754,89.8238053011624,90.8218475822865,91.8198898634105,
92.8179321445345,93.8159744256585,94.8140167067826,95.370521414155),
 .UNSPECIFIED.);
#404=B_SPLINE_CURVE_WITH_KNOTS('',3,(#13631,#13632,#13633,#13634,#13635,
#13636,#13637,#13638,#13639,#13640,#13641,#13642,#13643,#13644,#13645,#13646,
#13647,#13648,#13649,#13650,#13651,#13652),.UNSPECIFIED.,.F.,.F.,(4,3,3,
3,3,3,3,4),(-104.622988435322,-103.754857529378,-102.757214668519,-101.759571807659,
-100.7619289468,-99.7642860859406,-98.7666432250812,-98.3398031281424),
 .UNSPECIFIED.);
#405=B_SPLINE_CURVE_WITH_KNOTS('',3,(#13653,#13654,#13655,#13656,#13657,
#13658,#13659,#13660,#13661,#13662,#13663,#13664,#13665,#13666,#13667,#13668,
#13669,#13670,#13671,#13672,#13673,#13674),.UNSPECIFIED.,.F.,.F.,(4,3,3,
3,3,3,3,4),(95.370521414155,95.8120589879066,96.8101012690306,97.8081435501546,
98.8061858312787,99.8042281124027,100.802270393527,101.653706721335),
 .UNSPECIFIED.);
#406=B_SPLINE_CURVE_WITH_KNOTS('',3,(#13679,#13680,#13681,#13682,#13683,
#13684,#13685,#13686,#13687,#13688,#13689,#13690,#13691,#13692,#13693,#13694,
#13695,#13696,#13697,#13698,#13699,#13700,#13701,#13702,#13703),
 .UNSPECIFIED.,.F.,.F.,(4,3,3,3,3,3,3,3,4),(-110.906173742502,-110.738357555394,
-109.740714694535,-108.743071833675,-107.745428972816,-106.747786111956,
-105.750143251097,-104.752500390238,-104.622988435322),.UNSPECIFIED.);
#407=B_SPLINE_CURVE_WITH_KNOTS('',3,(#13704,#13705,#13706,#13707,#13708,
#13709,#13710,#13711,#13712,#13713,#13714,#13715,#13716,#13717,#13718,#13719,
#13720,#13721,#13722,#13723,#13724,#13725,#13726,#13727,#13728),
 .UNSPECIFIED.,.F.,.F.,(4,3,3,3,3,3,3,3,4),(101.653706721335,101.800312674651,
102.798354955775,103.796397236899,104.794439518023,105.792481799147,106.790524080271,
107.788566361395,107.936892028514),.UNSPECIFIED.);
#408=B_SPLINE_CURVE_WITH_KNOTS('',3,(#13733,#13734,#13735,#13736,#13737,
#13738,#13739,#13740,#13741,#13742,#13743,#13744,#13745,#13746,#13747,#13748,
#13749,#13750,#13751,#13752,#13753,#13754),.UNSPECIFIED.,.F.,.F.,(4,3,3,
3,3,3,3,4),(-117.189359049681,-116.724214720551,-115.726571859691,-114.728928998832,
-113.731286137972,-112.733643277113,-111.736000416253,-110.906173742502),
 .UNSPECIFIED.);
#409=B_SPLINE_CURVE_WITH_KNOTS('',3,(#13755,#13756,#13757,#13758,#13759,
#13760,#13761,#13762,#13763,#13764,#13765,#13766,#13767,#13768,#13769,#13770,
#13771,#13772,#13773,#13774,#13775,#13776),.UNSPECIFIED.,.F.,.F.,(4,3,3,
3,3,3,3,4),(107.936892028514,108.786608642519,109.784650923643,110.782693204767,
111.780735485891,112.778777767015,113.776820048139,114.220077335694),
 .UNSPECIFIED.);
#410=B_SPLINE_CURVE_WITH_KNOTS('',3,(#13781,#13782,#13783,#13784,#13785,
#13786,#13787,#13788,#13789,#13790,#13791,#13792,#13793,#13794,#13795,#13796,
#13797,#13798,#13799,#13800,#13801,#13802),.UNSPECIFIED.,.F.,.F.,(4,3,3,
3,3,3,3,4),(-123.472544356861,-122.710071885707,-121.712429024848,-120.714786163988,
-119.717143303129,-118.719500442269,-117.72185758141,-117.189359049681),
 .UNSPECIFIED.);
#411=B_SPLINE_CURVE_WITH_KNOTS('',3,(#13803,#13804,#13805,#13806,#13807,
#13808,#13809,#13810,#13811,#13812,#13813,#13814,#13815,#13816,#13817,#13818,
#13819,#13820,#13821,#13822,#13823,#13824),.UNSPECIFIED.,.F.,.F.,(4,3,3,
3,3,3,3,4),(114.220077335694,114.774862329263,115.772904610387,116.770946891511,
117.768989172635,118.767031453759,119.765073734883,120.503262642873),
 .UNSPECIFIED.);
#412=B_SPLINE_CURVE_WITH_KNOTS('',3,(#13829,#13830,#13831,#13832,#13833,
#13834,#13835,#13836,#13837,#13838,#13839,#13840,#13841,#13842,#13843,#13844,
#13845,#13846,#13847,#13848,#13849,#13850,#13851,#13852,#13853),
 .UNSPECIFIED.,.F.,.F.,(4,3,3,3,3,3,3,3,4),(-129.75572966404,-129.693571911723,
-128.695929050863,-127.698286190004,-126.700643329145,-125.703000468285,
-124.705357607426,-123.707714746566,-123.472544356861),.UNSPECIFIED.);
#413=B_SPLINE_CURVE_WITH_KNOTS('',3,(#13854,#13855,#13856,#13857,#13858,
#13859,#13860,#13861,#13862,#13863,#13864,#13865,#13866,#13867,#13868,#13869,
#13870,#13871,#13872,#13873,#13874,#13875,#13876,#13877,#13878),
 .UNSPECIFIED.,.F.,.F.,(4,3,3,3,3,3,3,3,4),(120.503262642873,120.763116016007,
121.761158297131,122.759200578255,123.757242859379,124.755285140503,125.753327421627,
126.751369702751,126.786447950053),.UNSPECIFIED.);
#414=B_SPLINE_CURVE_WITH_KNOTS('',3,(#13883,#13884,#13885,#13886,#13887,
#13888,#13889,#13890,#13891,#13892,#13893,#13894,#13895,#13896,#13897,#13898,
#13899,#13900,#13901,#13902,#13903,#13904),.UNSPECIFIED.,.F.,.F.,(4,3,3,
3,3,3,3,4),(-136.03891497122,-135.679429076879,-134.68178621602,-133.68414335516,
-132.686500494301,-131.688857633442,-130.691214772582,-129.75572966404),
 .UNSPECIFIED.);
#415=B_SPLINE_CURVE_WITH_KNOTS('',3,(#13905,#13906,#13907,#13908,#13909,
#13910,#13911,#13912,#13913,#13914,#13915,#13916,#13917,#13918,#13919,#13920,
#13921,#13922,#13923,#13924,#13925,#13926),.UNSPECIFIED.,.F.,.F.,(4,3,3,
3,3,3,3,4),(126.786447950053,127.749411983875,128.747454265,129.745496546124,
130.743538827248,131.741581108372,132.739623389496,133.069633257233),
 .UNSPECIFIED.);
#416=B_SPLINE_CURVE_WITH_KNOTS('',3,(#13931,#13932,#13933,#13934,#13935,
#13936,#13937,#13938,#13939,#13940,#13941,#13942,#13943,#13944,#13945,#13946,
#13947,#13948,#13949,#13950,#13951,#13952),.UNSPECIFIED.,.F.,.F.,(4,3,3,
3,3,3,3,4),(-142.322100278399,-141.665286242036,-140.667643381176,-139.670000520317,
-138.672357659457,-137.674714798598,-136.677071937739,-136.03891497122),
 .UNSPECIFIED.);
#417=B_SPLINE_CURVE_WITH_KNOTS('',3,(#13953,#13954,#13955,#13956,#13957,
#13958,#13959,#13960,#13961,#13962,#13963,#13964,#13965,#13966,#13967,#13968,
#13969,#13970,#13971,#13972,#13973,#13974),.UNSPECIFIED.,.F.,.F.,(4,3,3,
3,3,3,3,4),(133.069633257233,133.73766567062,134.735707951744,135.733750232868,
136.731792513992,137.729834795116,138.72787707624,139.352818564412),
 .UNSPECIFIED.);
#418=B_SPLINE_CURVE_WITH_KNOTS('',3,(#13979,#13980,#13981,#13982,#13983,
#13984,#13985,#13986,#13987,#13988,#13989,#13990,#13991,#13992,#13993,#13994,
#13995,#13996,#13997,#13998,#13999,#14000),.UNSPECIFIED.,.F.,.F.,(4,3,3,
3,3,3,3,4),(-148.605285585579,-147.651143407192,-146.653500546333,-145.655857685473,
-144.658214824614,-143.660571963754,-142.662929102895,-142.322100278399),
 .UNSPECIFIED.);
#419=B_SPLINE_CURVE_WITH_KNOTS('',3,(#14001,#14002,#14003,#14004,#14005,
#14006,#14007,#14008,#14009,#14010,#14011,#14012,#14013,#14014,#14015,#14016,
#14017,#14018,#14019,#14020,#14021,#14022),.UNSPECIFIED.,.F.,.F.,(4,3,3,
3,3,3,3,4),(139.352818564412,139.725919357364,140.723961638488,141.722003919612,
142.720046200736,143.71808848186,144.716130762984,145.636003871592),
 .UNSPECIFIED.);
#420=B_SPLINE_CURVE_WITH_KNOTS('',3,(#14027,#14028,#14029,#14030,#14031,
#14032,#14033,#14034,#14035,#14036,#14037,#14038,#14039,#14040,#14041,#14042,
#14043,#14044,#14045,#14046,#14047,#14048,#14049,#14050,#14051),
 .UNSPECIFIED.,.F.,.F.,(4,3,3,3,3,3,3,3,4),(-154.888470892759,-154.634643433208,
-153.637000572349,-152.639357711489,-151.64171485063,-150.64407198977,-149.646429128911,
-148.648786268052,-148.605285585579),.UNSPECIFIED.);
#421=B_SPLINE_CURVE_WITH_KNOTS('',3,(#14052,#14053,#14054,#14055,#14056,
#14057,#14058,#14059,#14060,#14061,#14062,#14063,#14064,#14065,#14066,#14067,
#14068,#14069,#14070,#14071,#14072,#14073,#14074,#14075,#14076),
 .UNSPECIFIED.,.F.,.F.,(4,3,3,3,3,3,3,3,4),(145.636003871592,145.714173044108,
146.712215325232,147.710257606356,148.70829988748,149.706342168604,150.704384449728,
151.702426730852,151.919189178771),.UNSPECIFIED.);
#422=B_SPLINE_CURVE_WITH_KNOTS('',3,(#14081,#14082,#14083,#14084,#14085,
#14086,#14087,#14088,#14089,#14090,#14091,#14092,#14093,#14094,#14095,#14096,
#14097,#14098,#14099,#14100,#14101,#14102),.UNSPECIFIED.,.F.,.F.,(4,3,3,
3,3,3,3,4),(-161.171656199938,-160.620500598364,-159.622857737505,-158.625214876646,
-157.627572015786,-156.629929154927,-155.632286294067,-154.888470892759),
 .UNSPECIFIED.);
#423=B_SPLINE_CURVE_WITH_KNOTS('',3,(#14103,#14104,#14105,#14106,#14107,
#14108,#14109,#14110,#14111,#14112,#14113,#14114,#14115,#14116,#14117,#14118,
#14119,#14120,#14121,#14122,#14123,#14124),.UNSPECIFIED.,.F.,.F.,(4,3,3,
3,3,3,3,4),(151.919189178771,152.700469011976,153.6985112931,154.696553574224,
155.694595855348,156.692638136472,157.690680417596,158.202374485951),
 .UNSPECIFIED.);
#424=B_SPLINE_CURVE_WITH_KNOTS('',3,(#14129,#14130,#14131,#14132,#14133,
#14134,#14135,#14136,#14137,#14138,#14139,#14140,#14141,#14142,#14143,#14144,
#14145,#14146,#14147,#14148,#14149,#14150),.UNSPECIFIED.,.F.,.F.,(4,3,3,
3,3,3,3,4),(-167.454841507118,-166.606357763521,-165.608714902661,-164.611072041802,
-163.613429180943,-162.615786320083,-161.618143459224,-161.171656199938),
 .UNSPECIFIED.);
#425=B_SPLINE_CURVE_WITH_KNOTS('',3,(#14151,#14152,#14153,#14154,#14155,
#14156,#14157,#14158,#14159,#14160,#14161,#14162,#14163,#14164,#14165,#14166,
#14167,#14168,#14169,#14170,#14171,#14172),.UNSPECIFIED.,.F.,.F.,(4,3,3,
3,3,3,3,4),(158.202374485951,158.68872269872,159.686764979844,160.684807260968,
161.682849542092,162.680891823216,163.67893410434,164.48555979313),
 .UNSPECIFIED.);
#426=B_SPLINE_CURVE_WITH_KNOTS('',3,(#14177,#14178,#14179,#14180,#14181,
#14182,#14183,#14184,#14185,#14186,#14187,#14188,#14189,#14190,#14191,#14192,
#14193,#14194,#14195,#14196,#14197,#14198,#14199,#14200,#14201),
 .UNSPECIFIED.,.F.,.F.,(4,3,3,3,3,3,3,3,4),(-173.738026814297,-173.589857789537,
-172.592214928677,-171.594572067818,-170.596929206958,-169.599286346099,
-168.60164348524,-167.60400062438,-167.454841507118),.UNSPECIFIED.);
#427=B_SPLINE_CURVE_WITH_KNOTS('',3,(#14202,#14203,#14204,#14205,#14206,
#14207,#14208,#14209,#14210,#14211,#14212,#14213,#14214,#14215,#14216,#14217,
#14218,#14219,#14220,#14221,#14222,#14223,#14224,#14225,#14226),
 .UNSPECIFIED.,.F.,.F.,(4,3,3,3,3,3,3,3,4),(164.48555979313,164.676976385465,
165.675018666588,166.673060947713,167.671103228837,168.669145509961,169.667187791085,
170.665230072209,170.76874510031),.UNSPECIFIED.);
#428=B_SPLINE_CURVE_WITH_KNOTS('',3,(#14231,#14232,#14233,#14234,#14235,
#14236,#14237,#14238,#14239,#14240,#14241,#14242,#14243,#14244,#14245,#14246,
#14247,#14248,#14249,#14250,#14251,#14252),.UNSPECIFIED.,.F.,.F.,(4,3,3,
3,3,3,3,4),(-180.021212121477,-179.575714954693,-178.578072093834,-177.580429232974,
-176.582786372115,-175.585143511255,-174.587500650396,-173.738026814297),
 .UNSPECIFIED.);
#429=B_SPLINE_CURVE_WITH_KNOTS('',3,(#14253,#14254,#14255,#14256,#14257,
#14258,#14259,#14260,#14261,#14262,#14263,#14264,#14265,#14266,#14267,#14268,
#14269,#14270,#14271,#14272,#14273,#14274),.UNSPECIFIED.,.F.,.F.,(4,3,3,
3,3,3,3,4),(170.76874510031,171.663272353333,172.661314634457,173.659356915581,
174.657399196705,175.655441477829,176.653483758953,177.051930407489),
 .UNSPECIFIED.);
#430=B_SPLINE_CURVE_WITH_KNOTS('',3,(#14279,#14280,#14281,#14282,#14283,
#14284,#14285,#14286,#14287,#14288,#14289,#14290,#14291,#14292,#14293,#14294,
#14295,#14296,#14297,#14298,#14299,#14300),.UNSPECIFIED.,.F.,.F.,(4,3,3,
3,3,3,3,4),(-186.304397428656,-185.56157211985,-184.56392925899,-183.566286398131,
-182.568643537271,-181.571000676412,-180.573357815553,-180.021212121477),
 .UNSPECIFIED.);
#431=B_SPLINE_CURVE_WITH_KNOTS('',3,(#14301,#14302,#14303,#14304,#14305,
#14306,#14307,#14308,#14309,#14310,#14311,#14312,#14313,#14314,#14315,#14316,
#14317,#14318,#14319,#14320,#14321,#14322),.UNSPECIFIED.,.F.,.F.,(4,3,3,
3,3,3,3,4),(177.051930407489,177.651526040077,178.649568321201,179.647610602325,
180.645652883449,181.643695164573,182.641737445697,183.335115714669),
 .UNSPECIFIED.);
#432=B_SPLINE_CURVE_WITH_KNOTS('',3,(#14328,#14329,#14330,#14331,#14332,
#14333,#14334,#14335,#14336,#14337),.UNSPECIFIED.,.F.,.F.,(4,1,1,1,1,1,
1,4),(197.920337176157,198.17515472821,199.172797589069,200.170440449928,
201.168083310788,202.165726171647,203.163369032507,204.161011893366),
 .UNSPECIFIED.);
#433=B_SPLINE_CURVE_WITH_KNOTS('',3,(#14340,#14341,#14342,#14343,#14344,
#14345,#14346,#14347,#14348),.UNSPECIFIED.,.F.,.F.,(4,1,1,1,1,1,4),(197.920337176157,
197.930069567874,198.928111848998,199.926154130122,200.924196411246,201.92223869237,
202.920280973494),.UNSPECIFIED.);
#434=B_SPLINE_CURVE_WITH_KNOTS('',3,(#14353,#14354,#14355,#14356,#14357,
#14358,#14359,#14360,#14361,#14362),.UNSPECIFIED.,.F.,.F.,(4,1,1,1,1,1,
1,4),(191.637151868977,192.189297563053,193.186940423913,194.184583284772,
195.182226145631,196.179869006491,197.17751186735,197.920337176157),
 .UNSPECIFIED.);
#435=B_SPLINE_CURVE_WITH_KNOTS('',3,(#14363,#14364,#14365,#14366,#14367,
#14368,#14369,#14370,#14371,#14372),.UNSPECIFIED.,.F.,.F.,(4,1,1,1,1,1,
1,4),(191.637151868977,191.94181588113,192.939858162254,193.937900443378,
194.935942724502,195.933985005626,196.93202728675,197.920337176157),
 .UNSPECIFIED.);
#436=B_SPLINE_CURVE_WITH_KNOTS('',3,(#14377,#14378,#14379,#14380,#14381,
#14382,#14383,#14384,#14385,#14386),.UNSPECIFIED.,.F.,.F.,(4,1,1,1,1,1,
1,4),(185.353966561798,186.203440397897,187.201083258756,188.198726119616,
189.196368980475,190.194011841334,191.191654702194,191.637151868977),
 .UNSPECIFIED.);
#437=B_SPLINE_CURVE_WITH_KNOTS('',3,(#14387,#14388,#14389,#14390,#14391,
#14392,#14393,#14394,#14395,#14396),.UNSPECIFIED.,.F.,.F.,(4,1,1,1,1,1,
1,4),(185.353966561798,185.953562194385,186.951604475509,187.949646756633,
188.947689037757,189.945731318881,190.943773600006,191.637151868977),
 .UNSPECIFIED.);
#438=B_SPLINE_CURVE_WITH_KNOTS('',3,(#14401,#14402,#14403,#14404,#14405,
#14406,#14407,#14408,#14409,#14410,#14411),.UNSPECIFIED.,.F.,.F.,(4,1,1,
1,1,1,1,1,4),(179.070781254618,179.219940371881,180.21758323274,181.2152260936,
182.212868954459,183.210511815318,184.208154676178,185.205797537037,185.353966561798),
 .UNSPECIFIED.);
#439=B_SPLINE_CURVE_WITH_KNOTS('',3,(#14412,#14413,#14414,#14415,#14416,
#14417,#14418,#14419,#14420,#14421),.UNSPECIFIED.,.F.,.F.,(4,1,1,1,1,1,
1,4),(179.070781254618,179.965308507641,180.963350788765,181.961393069889,
182.959435351013,183.957477632137,184.955519913261,185.353966561798),
 .UNSPECIFIED.);
#440=B_SPLINE_CURVE_WITH_KNOTS('',3,(#14426,#14427,#14428,#14429,#14430,
#14431,#14432,#14433,#14434,#14435),.UNSPECIFIED.,.F.,.F.,(4,1,1,1,1,1,
1,4),(172.787595947439,173.234083206724,174.231726067584,175.229368928443,
176.227011789303,177.224654650162,178.222297511021,179.070781254618),
 .UNSPECIFIED.);
#441=B_SPLINE_CURVE_WITH_KNOTS('',3,(#14436,#14437,#14438,#14439,#14440,
#14441,#14442,#14443,#14444,#14445,#14446),.UNSPECIFIED.,.F.,.F.,(4,1,1,
1,1,1,1,1,4),(172.787595947439,172.979012539773,173.977054820897,174.975097102021,
175.973139383145,176.971181664269,177.969223945393,178.967266226517,179.070781254618),
 .UNSPECIFIED.);
#442=B_SPLINE_CURVE_WITH_KNOTS('',3,(#14451,#14452,#14453,#14454,#14455,
#14456,#14457,#14458,#14459,#14460),.UNSPECIFIED.,.F.,.F.,(4,1,1,1,1,1,
1,4),(166.504410640259,167.248226041568,168.245868902427,169.243511763287,
170.241154624146,171.238797485006,172.236440345865,172.787595947439),
 .UNSPECIFIED.);
#443=B_SPLINE_CURVE_WITH_KNOTS('',3,(#14461,#14462,#14463,#14464,#14465,
#14466,#14467,#14468,#14469,#14470),.UNSPECIFIED.,.F.,.F.,(4,1,1,1,1,1,
1,4),(166.504410640259,166.990758853029,167.988801134153,168.986843415277,
169.984885696401,170.982927977525,171.980970258649,172.787595947439),
 .UNSPECIFIED.);
#444=B_SPLINE_CURVE_WITH_KNOTS('',3,(#14475,#14476,#14477,#14478,#14479,
#14480,#14481,#14482,#14483,#14484,#14485),.UNSPECIFIED.,.F.,.F.,(4,1,1,
1,1,1,1,1,4),(160.22122533308,160.264726015552,161.262368876412,162.260011737271,
163.25765459813,164.25529745899,165.252940319849,166.250583180709,166.504410640259),
 .UNSPECIFIED.);
#445=B_SPLINE_CURVE_WITH_KNOTS('',3,(#14486,#14487,#14488,#14489,#14490,
#14491,#14492,#14493,#14494,#14495),.UNSPECIFIED.,.F.,.F.,(4,1,1,1,1,1,
1,4),(160.22122533308,161.002505166285,162.000547447409,162.998589728533,
163.996632009657,164.994674290781,165.992716571905,166.504410640259),
 .UNSPECIFIED.);
#446=B_SPLINE_CURVE_WITH_KNOTS('',3,(#14500,#14501,#14502,#14503,#14504,
#14505,#14506,#14507,#14508,#14509),.UNSPECIFIED.,.F.,.F.,(4,1,1,1,1,1,
1,4),(153.9380400259,154.278868850396,155.276511711255,156.274154572115,
157.271797432974,158.269440293833,159.267083154693,160.22122533308),
 .UNSPECIFIED.);
#447=B_SPLINE_CURVE_WITH_KNOTS('',3,(#14510,#14511,#14512,#14513,#14514,
#14515,#14516,#14517,#14518,#14519,#14520),.UNSPECIFIED.,.F.,.F.,(4,1,1,
1,1,1,1,1,4),(153.9380400259,154.016209198417,155.014251479541,156.012293760665,
157.010336041789,158.008378322913,159.006420604037,160.004462885161,160.22122533308),
 .UNSPECIFIED.);
#448=B_SPLINE_CURVE_WITH_KNOTS('',3,(#14525,#14526,#14527,#14528,#14529,
#14530,#14531,#14532,#14533,#14534),.UNSPECIFIED.,.F.,.F.,(4,1,1,1,1,1,
1,4),(147.65485471872,148.293011685239,149.290654546099,150.288297406958,
151.285940267817,152.283583128677,153.281225989536,153.9380400259),
 .UNSPECIFIED.);
#449=B_SPLINE_CURVE_WITH_KNOTS('',3,(#14535,#14536,#14537,#14538,#14539,
#14540,#14541,#14542,#14543,#14544),.UNSPECIFIED.,.F.,.F.,(4,1,1,1,1,1,
1,4),(147.65485471872,148.027955511672,149.025997792796,150.02404007392,
151.022082355044,152.020124636168,153.018166917292,153.9380400259),
 .UNSPECIFIED.);
#450=B_SPLINE_CURVE_WITH_KNOTS('',3,(#14549,#14550,#14551,#14552,#14553,
#14554,#14555,#14556,#14557,#14558),.UNSPECIFIED.,.F.,.F.,(4,1,1,1,1,1,
1,4),(141.371669411541,142.307154520083,143.304797380942,144.302440241802,
145.300083102661,146.29772596352,147.29536882438,147.65485471872),
 .UNSPECIFIED.);
#451=B_SPLINE_CURVE_WITH_KNOTS('',3,(#14559,#14560,#14561,#14562,#14563,
#14564,#14565,#14566,#14567,#14568),.UNSPECIFIED.,.F.,.F.,(4,1,1,1,1,1,
1,4),(141.371669411541,142.039701824928,143.037744106052,144.035786387176,
145.0338286683,146.031870949424,147.029913230548,147.65485471872),
 .UNSPECIFIED.);
#452=B_SPLINE_CURVE_WITH_KNOTS('',3,(#14573,#14574,#14575,#14576,#14577,
#14578,#14579,#14580,#14581,#14582,#14583),.UNSPECIFIED.,.F.,.F.,(4,1,1,
1,1,1,1,1,4),(135.088484104361,135.323654494067,136.321297354926,137.318940215786,
138.316583076645,139.314225937505,140.311868798364,141.309511659223,141.371669411541),
 .UNSPECIFIED.);
#453=B_SPLINE_CURVE_WITH_KNOTS('',3,(#14584,#14585,#14586,#14587,#14588,
#14589,#14590,#14591,#14592,#14593),.UNSPECIFIED.,.F.,.F.,(4,1,1,1,1,1,
1,4),(135.088484104361,136.051448138184,137.049490419308,138.047532700432,
139.045574981556,140.04361726268,141.041659543804,141.371669411541),
 .UNSPECIFIED.);
#454=B_SPLINE_CURVE_WITH_KNOTS('',3,(#14598,#14599,#14600,#14601,#14602,
#14603,#14604,#14605,#14606,#14607),.UNSPECIFIED.,.F.,.F.,(4,1,1,1,1,1,
1,4),(128.805298797182,129.337797328911,130.33544018977,131.333083050629,
132.330725911489,133.328368772348,134.326011633208,135.088484104361),
 .UNSPECIFIED.);
#455=B_SPLINE_CURVE_WITH_KNOTS('',3,(#14608,#14609,#14610,#14611,#14612,
#14613,#14614,#14615,#14616,#14617,#14618),.UNSPECIFIED.,.F.,.F.,(4,1,1,
1,1,1,1,1,4),(128.805298797182,129.065152170316,130.06319445144,131.061236732564,
132.059279013688,133.057321294812,134.055363575936,135.05340585706,135.088484104361),
 .UNSPECIFIED.);
#456=B_SPLINE_CURVE_WITH_KNOTS('',3,(#14623,#14624,#14625,#14626,#14627,
#14628,#14629,#14630,#14631,#14632),.UNSPECIFIED.,.F.,.F.,(4,1,1,1,1,1,
1,4),(122.522113490002,123.351940163754,124.349583024614,125.347225885473,
126.344868746332,127.342511607192,128.340154468051,128.805298797182),
 .UNSPECIFIED.);
#457=B_SPLINE_CURVE_WITH_KNOTS('',3,(#14633,#14634,#14635,#14636,#14637,
#14638,#14639,#14640,#14641,#14642),.UNSPECIFIED.,.F.,.F.,(4,1,1,1,1,1,
1,4),(122.522113490002,123.076898483572,124.074940764696,125.07298304582,
126.071025326944,127.069067608068,128.067109889192,128.805298797182),
 .UNSPECIFIED.);
#458=B_SPLINE_CURVE_WITH_KNOTS('',3,(#14647,#14648,#14649,#14650,#14651,
#14652,#14653,#14654,#14655,#14656,#14657),.UNSPECIFIED.,.F.,.F.,(4,1,1,
1,1,1,1,1,4),(116.238928182823,116.368440137738,117.366082998598,118.363725859457,
119.361368720316,120.359011581176,121.356654442035,122.354297302895,122.522113490002),
 .UNSPECIFIED.);
#459=B_SPLINE_CURVE_WITH_KNOTS('',3,(#14658,#14659,#14660,#14661,#14662,
#14663,#14664,#14665,#14666,#14667),.UNSPECIFIED.,.F.,.F.,(4,1,1,1,1,1,
1,4),(116.238928182823,117.088644796828,118.086687077952,119.084729359076,
120.0827716402,121.080813921324,122.078856202448,122.522113490002),
 .UNSPECIFIED.);
#460=B_SPLINE_CURVE_WITH_KNOTS('',3,(#14672,#14673,#14674,#14675,#14676,
#14677,#14678,#14679,#14680,#14681),.UNSPECIFIED.,.F.,.F.,(4,1,1,1,1,1,
1,4),(109.955742875643,110.382582972582,111.380225833441,112.377868694301,
113.37551155516,114.373154416019,115.370797276879,116.238928182823),
 .UNSPECIFIED.);
#461=B_SPLINE_CURVE_WITH_KNOTS('',3,(#14682,#14683,#14684,#14685,#14686,
#14687,#14688,#14689,#14690,#14691,#14692),.UNSPECIFIED.,.F.,.F.,(4,1,1,
1,1,1,1,1,4),(109.955742875643,110.102348828959,111.100391110083,112.098433391207,
113.096475672331,114.094517953455,115.092560234579,116.090602515703,116.238928182823),
 .UNSPECIFIED.);
#462=B_SPLINE_CURVE_WITH_KNOTS('',3,(#14697,#14698,#14699,#14700,#14701,
#14702,#14703,#14704,#14705,#14706),.UNSPECIFIED.,.F.,.F.,(4,1,1,1,1,1,
1,4),(103.672557568463,104.396725807425,105.394368668285,106.392011529144,
107.389654390004,108.387297250863,109.384940111722,109.955742875643),
 .UNSPECIFIED.);
#463=B_SPLINE_CURVE_WITH_KNOTS('',3,(#14707,#14708,#14709,#14710,#14711,
#14712,#14713,#14714,#14715,#14716),.UNSPECIFIED.,.F.,.F.,(4,1,1,1,1,1,
1,4),(103.672557568463,104.114095142215,105.112137423339,106.110179704463,
107.108221985587,108.106264266711,109.104306547835,109.955742875643),
 .UNSPECIFIED.);
#464=B_SPLINE_CURVE_WITH_KNOTS('',3,(#14721,#14722,#14723,#14724,#14725,
#14726,#14727,#14728,#14729,#14730,#14731),.UNSPECIFIED.,.F.,.F.,(4,1,1,
1,1,1,1,1,4),(97.3893722612837,97.4132257814096,98.410868642269,99.4085115031284,
100.406154363988,101.403797224847,102.401440085707,103.399082946566,103.672557568463),
 .UNSPECIFIED.);
#465=B_SPLINE_CURVE_WITH_KNOTS('',3,(#14732,#14733,#14734,#14735,#14736,
#14737,#14738,#14739,#14740,#14741),.UNSPECIFIED.,.F.,.F.,(4,1,1,1,1,1,
1,4),(97.3893722612838,98.125841455471,99.123883736595,100.121926017719,
101.119968298843,102.118010579967,103.116052861091,103.672557568463),
 .UNSPECIFIED.);
#466=B_SPLINE_CURVE_WITH_KNOTS('',3,(#14746,#14747,#14748,#14749,#14750,
#14751,#14752,#14753,#14754,#14755),.UNSPECIFIED.,.F.,.F.,(4,1,1,1,1,1,
1,4),(91.1061869541041,91.4273686162531,92.4250114771125,93.4226543379719,
94.4202971988313,95.4179400596907,96.4155829205502,97.3893722612837),
 .UNSPECIFIED.);
#467=B_SPLINE_CURVE_WITH_KNOTS('',3,(#14756,#14757,#14758,#14759,#14760,
#14761,#14762,#14763,#14764,#14765,#14766),.UNSPECIFIED.,.F.,.F.,(4,1,1,
1,1,1,1,1,4),(91.1061869541042,91.1395454876028,92.1375877687268,93.1356300498508,
94.1336723309749,95.1317146120989,96.1297568932229,97.127799174347,97.3893722612838),
 .UNSPECIFIED.);
#468=B_SPLINE_CURVE_WITH_KNOTS('',3,(#14771,#14772,#14773,#14774,#14775,
#14776,#14777,#14778,#14779,#14780),.UNSPECIFIED.,.F.,.F.,(4,1,1,1,1,1,
1,4),(84.8230016469245,85.4415114510967,86.4391543119561,87.4367971728155,
88.4344400336749,89.4320828945343,90.4297257553937,91.1061869541041),
 .UNSPECIFIED.);
#469=B_SPLINE_CURVE_WITH_KNOTS('',3,(#14781,#14782,#14783,#14784,#14785,
#14786,#14787,#14788,#14789,#14790),.UNSPECIFIED.,.F.,.F.,(4,1,1,1,1,1,
1,4),(84.8230016469246,85.1512918008586,86.1493340819827,87.1473763631067,
88.1454186442307,89.1434609253548,90.1415032064788,91.1061869541042),
 .UNSPECIFIED.);
#470=B_SPLINE_CURVE_WITH_KNOTS('',3,(#14795,#14796,#14797,#14798,#14799,
#14800,#14801,#14802,#14803,#14804),.UNSPECIFIED.,.F.,.F.,(4,1,1,1,1,1,
1,4),(78.539816339745,79.4556542859402,80.4532971467996,81.4509400076591,
82.4485828685185,83.4462257293779,84.4438685902373,84.8230016469245),
 .UNSPECIFIED.);
#471=B_SPLINE_CURVE_WITH_KNOTS('',3,(#14805,#14806,#14807,#14808,#14809,
#14810,#14811,#14812,#14813,#14814),.UNSPECIFIED.,.F.,.F.,(4,1,1,1,1,1,
1,4),(78.539816339745,79.1630381141145,80.1610803952385,81.1591226763625,
82.1571649574865,83.1552072386106,84.1532495197346,84.8230016469246),
 .UNSPECIFIED.);
#472=B_SPLINE_CURVE_WITH_KNOTS('',3,(#14819,#14820,#14821,#14822,#14823,
#14824,#14825,#14826,#14827,#14828,#14829),.UNSPECIFIED.,.F.,.F.,(4,1,1,
1,1,1,1,1,4),(72.2566310325654,72.4721542599244,73.4697971207838,74.4674399816432,
75.4650828425026,76.462725703362,77.4603685642214,78.4580114250808,78.539816339745),
 .UNSPECIFIED.);
#473=B_SPLINE_CURVE_WITH_KNOTS('',3,(#14830,#14831,#14832,#14833,#14834,
#14835,#14836,#14837,#14838,#14839),.UNSPECIFIED.,.F.,.F.,(4,1,1,1,1,1,
1,4),(72.2566310325654,73.1747844273703,74.1728267084943,75.1708689896184,
76.1689112707424,77.1669535518664,78.1649958329905,78.539816339745),
 .UNSPECIFIED.);
#474=B_SPLINE_CURVE_WITH_KNOTS('',3,(#14844,#14845,#14846,#14847,#14848,
#14849,#14850,#14851,#14852,#14853),.UNSPECIFIED.,.F.,.F.,(4,1,1,1,1,1,
1,4),(65.9734457253858,66.486297094768,67.4839399556274,68.4815828164868,
69.4792256773462,70.4768685382056,71.474511399065,72.2566310325654),
 .UNSPECIFIED.);
#475=B_SPLINE_CURVE_WITH_KNOTS('',3,(#14854,#14855,#14856,#14857,#14858,
#14859,#14860,#14861,#14862,#14863,#14864),.UNSPECIFIED.,.F.,.F.,(4,1,1,
1,1,1,1,1,4),(65.9734457253858,66.1884884595021,67.1865307406262,68.1845730217502,
69.1826153028742,70.1806575839982,71.1786998651223,72.1767421462463,72.2566310325654),
 .UNSPECIFIED.);
#476=B_SPLINE_CURVE_WITH_KNOTS('',3,(#14869,#14870,#14871,#14872,#14873,
#14874,#14875,#14876,#14877,#14878),.UNSPECIFIED.,.F.,.F.,(4,1,1,1,1,1,
1,4),(59.6902604182062,60.5004399296115,61.4980827904709,62.4957256513303,
63.4933685121897,64.4910113730492,65.4886542339086,65.9734457253858),
 .UNSPECIFIED.);
#477=B_SPLINE_CURVE_WITH_KNOTS('',3,(#14879,#14880,#14881,#14882,#14883,
#14884,#14885,#14886,#14887,#14888),.UNSPECIFIED.,.F.,.F.,(4,1,1,1,1,1,
1,4),(59.6902604182062,60.200234772758,61.198277053882,62.196319335006,
63.19436161613,64.1924038972541,65.1904461783781,65.9734457253858),
 .UNSPECIFIED.);
#478=B_SPLINE_CURVE_WITH_KNOTS('',3,(#14893,#14894,#14895,#14896,#14897,
#14898,#14899,#14900,#14901,#14902,#14903),.UNSPECIFIED.,.F.,.F.,(4,1,1,
1,1,1,1,1,4),(53.4070751110266,53.5169399035957,54.5145827644551,55.5122256253145,
56.5098684861739,57.5075113470333,58.5051542078927,59.5027970687521,59.6902604182062),
 .UNSPECIFIED.);
#479=B_SPLINE_CURVE_WITH_KNOTS('',3,(#14904,#14905,#14906,#14907,#14908,
#14909,#14910,#14911,#14912,#14913),.UNSPECIFIED.,.F.,.F.,(4,1,1,1,1,1,
1,4),(53.4070751110266,54.2119810860138,55.2100233671378,56.2080656482619,
57.2061079293859,58.2041502105099,59.2021924916339,59.6902604182062),
 .UNSPECIFIED.);
#480=B_SPLINE_CURVE_WITH_KNOTS('',3,(#14918,#14919,#14920,#14921,#14922,
#14923,#14924,#14925,#14926,#14927),.UNSPECIFIED.,.F.,.F.,(4,1,1,1,1,1,
1,4),(47.123889803847,47.5310827384393,48.5287255992987,49.5263684601581,
50.5240113210175,51.5216541818769,52.5192970427363,53.4070751110266),
 .UNSPECIFIED.);
#481=B_SPLINE_CURVE_WITH_KNOTS('',3,(#14928,#14929,#14930,#14931,#14932,
#14933,#14934,#14935,#14936,#14937,#14938),.UNSPECIFIED.,.F.,.F.,(4,1,1,
1,1,1,1,1,4),(47.123889803847,47.2256851181456,48.2237273992696,49.2217696803937,
50.2198119615177,51.2178542426417,52.2158965237657,53.2139388048898,53.4070751110266),
 .UNSPECIFIED.);
#482=B_SPLINE_CURVE_WITH_KNOTS('',3,(#14943,#14944,#14945,#14946,#14947,
#14948,#14949,#14950,#14951,#14952),.UNSPECIFIED.,.F.,.F.,(4,1,1,1,1,1,
1,4),(40.8407044966674,41.5452255732828,42.5428684341422,43.5405112950016,
44.538154155861,45.5357970167204,46.5334398775799,47.123889803847),
 .UNSPECIFIED.);
#483=B_SPLINE_CURVE_WITH_KNOTS('',3,(#14953,#14954,#14955,#14956,#14957,
#14958,#14959,#14960,#14961,#14962),.UNSPECIFIED.,.F.,.F.,(4,1,1,1,1,1,
1,4),(40.8407044966675,41.2374314314014,42.2354737125255,43.2335159936495,
44.2315582747735,45.2296005558975,46.2276428370216,47.123889803847),
 .UNSPECIFIED.);
#484=B_SPLINE_CURVE_WITH_KNOTS('',3,(#14967,#14968,#14969,#14970,#14971,
#14972,#14973,#14974,#14975,#14976,#14977),.UNSPECIFIED.,.F.,.F.,(4,1,1,
1,1,1,1,1,4),(34.5575191894878,34.561725547267,35.5593684081264,36.5570112689858,
37.5546541298452,38.5522969907046,39.549939851564,40.5475827124234,40.8407044966674),
 .UNSPECIFIED.);
#485=B_SPLINE_CURVE_WITH_KNOTS('',3,(#14978,#14979,#14980,#14981,#14982,
#14983,#14984,#14985,#14986,#14987),.UNSPECIFIED.,.F.,.F.,(4,1,1,1,1,1,
1,4),(34.5575191894879,35.2491777446573,36.2472200257813,37.2452623069053,
38.2433045880294,39.2413468691534,40.2393891502774,40.8407044966675),
 .UNSPECIFIED.);
#486=B_SPLINE_CURVE_WITH_KNOTS('',3,(#14992,#14993,#14994,#14995,#14996,
#14997,#14998,#14999,#15000,#15001),.UNSPECIFIED.,.F.,.F.,(4,1,1,1,1,1,
1,4),(28.2743338823082,28.5758683821105,29.5735112429699,30.5711541038294,
31.5687969646888,32.5664398255482,33.5640826864076,34.5575191894878),
 .UNSPECIFIED.);
#487=B_SPLINE_CURVE_WITH_KNOTS('',3,(#15002,#15003,#15004,#15005,#15006,
#15007,#15008,#15009,#15010,#15011),.UNSPECIFIED.,.F.,.F.,(4,1,1,1,1,1,
1,4),(28.2743338823083,29.2609240579131,30.2589663390371,31.2570086201612,
32.2550509012852,33.2530931824092,34.2511354635333,34.5575191894879),
 .UNSPECIFIED.);
#488=B_SPLINE_CURVE_WITH_KNOTS('',3,(#15016,#15017,#15018,#15019,#15020,
#15021,#15022,#15023,#15024,#15025),.UNSPECIFIED.,.F.,.F.,(4,1,1,1,1,1,
1,4),(21.9911485751286,22.5900112169541,23.5876540778135,24.5852969386729,
25.5829397995323,26.5805826603917,27.5782255212511,28.2743338823082),
 .UNSPECIFIED.);
#489=B_SPLINE_CURVE_WITH_KNOTS('',3,(#15026,#15027,#15028,#15029,#15030,
#15031,#15032,#15033,#15034,#15035,#15036),.UNSPECIFIED.,.F.,.F.,(4,1,1,
1,1,1,1,1,4),(21.9911485751287,22.2746280900449,23.272670371169,24.270712652293,
25.268754933417,26.266797214541,27.2648394956651,28.2628817767891,28.2743338823083),
 .UNSPECIFIED.);
#490=B_SPLINE_CURVE_WITH_KNOTS('',3,(#15041,#15042,#15043,#15044,#15045,
#15046,#15047,#15048,#15049,#15050),.UNSPECIFIED.,.F.,.F.,(4,1,1,1,1,1,
1,4),(15.707963267949,16.6041540517977,17.6017969126571,18.5994397735165,
19.5970826343759,20.5947254952353,21.5923683560947,21.9911485751286),
 .UNSPECIFIED.);
#491=B_SPLINE_CURVE_WITH_KNOTS('',3,(#15051,#15052,#15053,#15054,#15055,
#15056,#15057,#15058,#15059,#15060),.UNSPECIFIED.,.F.,.F.,(4,1,1,1,1,1,
1,4),(15.7079632679491,16.2863744033008,17.2844166844248,18.2824589655488,
19.2805012466728,20.2785435277969,21.2765858089209,21.9911485751287),
 .UNSPECIFIED.);
#492=B_SPLINE_CURVE_WITH_KNOTS('',3,(#15063,#15064,#15065,#15066,#15067,
#15068,#15069,#15070,#15071,#15072,#15073,#15074,#15075,#15076,#15077,#15078,
#15079,#15080,#15081,#15082,#15083,#15084,#15085,#15086,#15087,#15088,#15089,
#15090,#15091,#15092,#15093,#15094,#15095,#15096,#15097,#15098,#15099,#15100,
#15101,#15102,#15103,#15104,#15105,#15106,#15107,#15108,#15109,#15110,#15111,
#15112,#15113,#15114,#15115,#15116,#15117,#15118,#15119,#15120,#15121,#15122,
#15123,#15124,#15125,#15126,#15127,#15128,#15129,#15130,#15131,#15132,#15133,
#15134,#15135,#15136,#15137,#15138,#15139,#15140,#15141,#15142,#15143,#15144,
#15145,#15146,#15147,#15148,#15149,#15150,#15151,#15152,#15153,#15154,#15155,
#15156,#15157,#15158,#15159,#15160,#15161,#15162,#15163,#15164,#15165,#15166,
#15167,#15168,#15169,#15170,#15171,#15172,#15173,#15174,#15175,#15176,#15177,
#15178,#15179,#15180,#15181,#15182,#15183),.UNSPECIFIED.,.F.,.F.,(4,3,3,
3,3,3,3,3,3,3,3,3,3,3,3,3,3,3,3,3,3,3,3,3,3,3,3,3,3,3,3,3,3,3,3,3,3,3,3,
3,4),(-0.753008129282056,-0.726412283548368,-0.715911613874471,-0.694893371653716,
-0.683361029549332,-0.673826434412814,-0.652889016486892,-0.639679181765185,
-0.63195159856097,-0.60480408471638,-0.59150990338668,-0.582561183693184,
-0.554067746128576,-0.540494882749548,-0.528208608719221,-0.505843484121927,
-0.4921308028701,-0.483102814228457,-0.456032674248847,-0.436199115577779,
-0.427073928162626,-0.400948091236321,-0.382860905241332,-0.374822254310016,
-0.34584221065474,-0.333939649620793,-0.324058619604945,-0.29393738163796,
-0.278576588250954,-0.269234263278142,-0.238815915606663,-0.225742435796944,
-0.216239773488962,-0.18666367230127,-0.170750005528772,-0.161294486761502,
-0.129614927749849,-0.114924930935507,-0.106250072717365,-0.0979353687381955,
-0.0965360155478562),.UNSPECIFIED.);
#493=B_SPLINE_CURVE_WITH_KNOTS('',3,(#15185,#15186,#15187,#15188,#15189,
#15190,#15191,#15192,#15193,#15194,#15195,#15196,#15197,#15198,#15199,#15200,
#15201,#15202,#15203,#15204,#15205,#15206,#15207,#15208,#15209,#15210,#15211,
#15212,#15213,#15214,#15215,#15216,#15217,#15218,#15219,#15220,#15221),
 .UNSPECIFIED.,.F.,.F.,(4,3,3,3,3,3,3,3,3,3,3,3,4),(-0.204609524178132,
-0.173922074105667,-0.152149392827302,-0.142793959810126,-0.12983323009626,
-0.11308637627832,-0.0998536142809363,-0.090547498816978,-0.0679106241127335,
-0.0514558350659385,-0.042025593252969,-0.0155529233063705,0.),
 .UNSPECIFIED.);
#494=B_SPLINE_CURVE_WITH_KNOTS('',3,(#15224,#15225,#15226,#15227,#15228,
#15229,#15230,#15231,#15232,#15233,#15234,#15235,#15236,#15237,#15238,#15239),
 .UNSPECIFIED.,.F.,.F.,(4,3,3,3,3,4),(-0.0965360155478562,-0.0724020116608921,
-0.0590232605257019,-0.050388474335024,-0.0186937936910934,0.),
 .UNSPECIFIED.);
#495=B_SPLINE_CURVE_WITH_KNOTS('',3,(#16028,#16029,#16030,#16031,#16032,
#16033,#16034,#16035),.UNSPECIFIED.,.F.,.F.,(4,1,1,1,1,4),(11.6159397475006,
12.61358260836,13.6112254692194,14.6088683300789,15.6065111909383,15.707963267949),
 .UNSPECIFIED.);
#496=B_SPLINE_CURVE_WITH_KNOTS('',3,(#16036,#16037,#16038,#16039,#16040,
#16041,#16042,#16043,#16044,#16045,#16046,#16047,#16048,#16049,#16050,#16051,
#16052,#16053,#16054,#16055,#16056,#16057,#16058,#16059,#16060,#16061,#16062,
#16063,#16064,#16065,#16066,#16067,#16068,#16069,#16070,#16071,#16072,#16073,
#16074,#16075,#16076,#16077,#16078,#16079,#16080,#16081,#16082,#16083,#16084),
 .UNSPECIFIED.,.F.,.F.,(4,3,3,3,3,3,3,3,3,3,3,3,3,3,3,3,4),(-0.275362278356892,
-0.263988733943187,-0.242277787653762,-0.228409792083558,-0.208856161945484,
-0.197709057767663,-0.168075464588018,-0.150222803571495,-0.140083955862437,
-0.125365894046572,-0.0997819296507484,-0.0889593225835958,-0.0667194919376969,
-0.0511923416312717,-0.0404361839568205,-0.0141940669149386,0.),
 .UNSPECIFIED.);
#497=B_SPLINE_CURVE_WITH_KNOTS('',3,(#16085,#16086,#16087,#16088,#16089,
#16090,#16091,#16092,#16093,#16094,#16095,#16096,#16097,#16098,#16099,#16100,
#16101,#16102,#16103),.UNSPECIFIED.,.F.,.F.,(4,3,3,3,3,3,4),(-191.027404416132,
-190.549786424147,-189.552143563287,-188.554500702428,-187.556857841568,
-186.559214980709,-186.304397428656),.UNSPECIFIED.);
#498=B_SPLINE_CURVE_WITH_KNOTS('',3,(#16106,#16107,#16108,#16109,#16110,
#16111,#16112,#16113,#16114),.UNSPECIFIED.,.F.,.F.,(4,1,1,1,1,1,4),(10.3752088276283,
11.2961629976806,12.2942052788047,13.2922475599287,14.2902898410527,15.2883321221767,
15.7079632679491),.UNSPECIFIED.);
#499=B_SPLINE_CURVE_WITH_KNOTS('',3,(#16908,#16909,#16910,#16911,#16912,
#16913,#16914,#16915,#16916,#16917,#16918,#16919,#16920,#16921,#16922,#16923,
#16924,#16925,#16926,#16927,#16928,#16929),.UNSPECIFIED.,.F.,.F.,(4,3,3,
3,3,3,3,4),(183.335115714669,183.639779726821,184.637822007945,185.635864289069,
186.633906570193,187.631948851317,188.629991132441,188.954231742812),
 .UNSPECIFIED.);
#500=B_SPLINE_CURVE_WITH_KNOTS('',3,(#16930,#16931,#16932,#16933,#16934,
#16935,#16936,#16937,#16938,#16939,#16940,#16941,#16942,#16943,#16944,#16945,
#16946,#16947,#16948,#16949,#16950,#16951,#16952,#16953,#16954,#16955,#16956,
#16957,#16958,#16959,#16960,#16961,#16962,#16963,#16964,#16965,#16966,#16967,
#16968,#16969,#16970,#16971,#16972,#16973,#16974,#16975,#16976,#16977,#16978,
#16979,#16980,#16981),.UNSPECIFIED.,.F.,.F.,(4,3,3,3,3,3,3,3,3,3,3,3,3,
3,3,3,3,4),(-0.276631791712714,-0.267404104599176,-0.245529112929484,-0.233826742508505,
-0.212230201958684,-0.201819484750363,-0.173281546649687,-0.162756755581661,
-0.152537502224722,-0.140478169692516,-0.120739781640826,-0.110641775261762,
-0.100726383882944,-0.0755447879122082,-0.0587891884452614,-0.0493012364577666,
-0.0182848522583483,0.),.UNSPECIFIED.);
#501=B_SPLINE_CURVE_WITH_KNOTS('',3,(#17036,#17037,#17038,#17039,#17040,
#17041,#17042),.UNSPECIFIED.,.F.,.F.,(4,3,4),(-30.159289474462,-29.2544199692899,
-28.9853432330879),.UNSPECIFIED.);
#502=B_SPLINE_CURVE_WITH_KNOTS('',3,(#17048,#17049,#17050,#17051,#17052,
#17053,#17054,#17055,#17056,#17057,#17058,#17059,#17060,#17061,#17062,#17063,
#17064,#17065,#17066),.UNSPECIFIED.,.F.,.F.,(4,3,3,3,3,3,4),(26.4423043696954,
27.3041253046706,28.2792726369803,29.25441996929,30.2295673015996,31.2047146339093,
32.179861966219),.UNSPECIFIED.);
#503=B_SPLINE_CURVE_WITH_KNOTS('',3,(#17068,#17069,#17070,#17071,#17072,
#17073,#17074,#17075,#17076,#17077,#17078,#17079,#17080,#17081,#17082,#17083,
#17084,#17085,#17086,#17087,#17088,#17089),.UNSPECIFIED.,.F.,.F.,(4,3,3,
3,3,3,3,4),(-28.9853432330879,-28.2792726369803,-27.3041253046706,-26.3289779723609,
-25.3538306400513,-24.3786833077416,-23.403535975432,-22.7021579259084),
 .UNSPECIFIED.);
#504=B_SPLINE_CURVE_WITH_KNOTS('',3,(#17094,#17095,#17096,#17097,#17098,
#17099,#17100,#17101,#17102,#17103,#17104,#17105,#17106,#17107,#17108,#17109,
#17110,#17111,#17112,#17113,#17114,#17115,#17116,#17117,#17118),
 .UNSPECIFIED.,.F.,.F.,(4,3,3,3,3,3,3,3,4),(20.1591190625159,20.478093978503,
21.4532413108126,22.4283886431223,23.403535975432,24.3786833077416,25.3538306400513,
26.328977972361,26.4423043696954),.UNSPECIFIED.);
#505=B_SPLINE_CURVE_WITH_KNOTS('',3,(#17119,#17120,#17121,#17122,#17123,
#17124,#17125,#17126,#17127,#17128,#17129,#17130,#17131,#17132,#17133,#17134,
#17135,#17136,#17137,#17138,#17139,#17140,#17141,#17142,#17143),
 .UNSPECIFIED.,.F.,.F.,(4,3,3,3,3,3,3,3,4),(-22.7021579259084,-22.4283886431223,
-21.4532413108126,-20.478093978503,-19.5029466461933,-18.5277993138836,
-17.552651981574,-16.5775046492643,-16.4189726187288),.UNSPECIFIED.);
#506=B_SPLINE_CURVE_WITH_KNOTS('',3,(#17148,#17149,#17150,#17151,#17152,
#17153,#17154,#17155,#17156,#17157,#17158,#17159,#17160,#17161,#17162,#17163,
#17164,#17165,#17166,#17167,#17168,#17169),.UNSPECIFIED.,.F.,.F.,(4,3,3,
3,3,3,3,4),(13.8759337553363,14.627209984645,15.6023573169546,16.5775046492643,
17.552651981574,18.5277993138836,19.5029466461933,20.1591190625159),
 .UNSPECIFIED.);
#507=B_SPLINE_CURVE_WITH_KNOTS('',3,(#17170,#17171,#17172,#17173,#17174,
#17175,#17176,#17177,#17178,#17179,#17180,#17181,#17182,#17183,#17184,#17185,
#17186,#17187,#17188,#17189,#17190,#17191),.UNSPECIFIED.,.F.,.F.,(4,3,3,
3,3,3,3,4),(-16.4189726187288,-15.6023573169546,-14.627209984645,-13.6520626523353,
-12.6769153200256,-11.701767987716,-10.7266206554063,-10.1357873115492),
 .UNSPECIFIED.);
#508=B_SPLINE_CURVE_WITH_KNOTS('',3,(#17197,#17198,#17199,#17200,#17201,
#17202,#17203,#17204,#17205,#17206,#17207,#17208,#17209),.UNSPECIFIED.,
 .F.,.F.,(4,3,3,3,4),(-3.8526020043696,-2.92544199692899,-1.95029466461933,
-0.975147332309664,0.),.UNSPECIFIED.);
#509=B_SPLINE_CURVE_WITH_KNOTS('',3,(#17212,#17213,#17214,#17215,#17216,
#17217,#17218,#17219,#17220,#17221,#17222,#17223,#17224,#17225,#17226,#17227,
#17228,#17229,#17230),.UNSPECIFIED.,.F.,.F.,(4,3,3,3,3,3,4),(2.02057249175693,
2.925441996929,3.90058932923866,4.87573666154832,5.85088399385799,6.82603132616766,
7.59274844815668),.UNSPECIFIED.);
#510=B_SPLINE_CURVE_WITH_KNOTS('',3,(#17236,#17237,#17238,#17239,#17240,
#17241,#17242),.UNSPECIFIED.,.F.,.F.,(4,1,1,1,4),(40.8407044966673,41.1097812328693,
42.084928565179,43.0600758974886,44.0352232297983),.UNSPECIFIED.);
#511=B_SPLINE_CURVE_WITH_KNOTS('',3,(#17245,#17246,#17247,#17248,#17249,
#17250,#17251),.UNSPECIFIED.,.F.,.F.,(4,1,1,1,4),(40.8407044966673,41.7025254316425,
42.6776727639522,43.6528200962618,44.5576896014339),.UNSPECIFIED.);
#512=B_SPLINE_CURVE_WITH_KNOTS('',3,(#17256,#17257,#17258,#17259,#17260,
#17261,#17262,#17263,#17264,#17265),.UNSPECIFIED.,.F.,.F.,(4,1,1,1,1,1,
1,4),(34.5575191894877,35.2588972390113,36.234044571321,37.2091919036307,
38.1843392359403,39.15948656825,40.1346339005596,40.8407044966673),
 .UNSPECIFIED.);
#513=B_SPLINE_CURVE_WITH_KNOTS('',3,(#17266,#17267,#17268,#17269,#17270,
#17271,#17272,#17273,#17274,#17275,#17276),.UNSPECIFIED.,.F.,.F.,(4,1,1,
1,1,1,1,1,4),(34.5575191894877,34.8764941054748,35.8516414377845,36.8267887700942,
37.8019361024038,38.7770834347135,39.7522307670232,40.7273780993328,40.8407044966673),
 .UNSPECIFIED.);
#514=B_SPLINE_CURVE_WITH_KNOTS('',3,(#17281,#17282,#17283,#17284,#17285,
#17286,#17287,#17288,#17289,#17290,#17291),.UNSPECIFIED.,.F.,.F.,(4,1,1,
1,1,1,1,1,4),(28.2743338823081,28.4328659128437,29.4080132451533,30.383160577463,
31.3583079097727,32.3334552420823,33.308602574392,34.2837499067017,34.5575191894877),
 .UNSPECIFIED.);
#515=B_SPLINE_CURVE_WITH_KNOTS('',3,(#17292,#17293,#17294,#17295,#17296,
#17297,#17298,#17299,#17300,#17301),.UNSPECIFIED.,.F.,.F.,(4,1,1,1,1,1,
1,4),(28.2743338823081,29.0256101116168,30.0007574439265,30.9759047762362,
31.9510521085458,32.9261994408555,33.9013467731652,34.5575191894877),
 .UNSPECIFIED.);
#516=B_SPLINE_CURVE_WITH_KNOTS('',3,(#17306,#17307,#17308,#17309,#17310,
#17311,#17312,#17313,#17314,#17315),.UNSPECIFIED.,.F.,.F.,(4,1,1,1,1,1,
1,4),(21.9911485751285,22.5819819189857,23.5571292512954,24.532276583605,
25.5074239159147,26.4825712482243,27.457718580534,28.2743338823081),
 .UNSPECIFIED.);
#517=B_SPLINE_CURVE_WITH_KNOTS('',3,(#17316,#17317,#17318,#17319,#17320,
#17321,#17322,#17323,#17324,#17325,#17326),.UNSPECIFIED.,.F.,.F.,(4,1,1,
1,1,1,1,1,4),(21.9911485751285,22.1995787854492,23.1747261177589,24.1498734500685,
25.1250207823782,26.1001681146879,27.0753154469975,28.0504627793072,28.2743338823081),
 .UNSPECIFIED.);
#518=B_SPLINE_CURVE_WITH_KNOTS('',3,(#17332,#17333,#17334,#17335,#17336),
 .UNSPECIFIED.,.F.,.F.,(4,1,4),(14.3984001269719,15.3735474592815,15.7079632679489),
 .UNSPECIFIED.);
#519=B_SPLINE_CURVE_WITH_KNOTS('',3,(#17339,#17340,#17341,#17342,#17343),
 .UNSPECIFIED.,.F.,.F.,(4,1,4),(13.8759337553363,14.7808032605084,15.7079632679489),
 .UNSPECIFIED.);
#520=B_SPLINE_CURVE_WITH_KNOTS('',3,(#17345,#17346,#17347,#17348,#17349,
#17350,#17351,#17352,#17353,#17354,#17355),.UNSPECIFIED.,.F.,.F.,(4,1,1,
1,1,1,1,1,4),(15.7079632679489,15.755950592818,16.7310979251277,17.7062452574374,
18.681392589747,19.6565399220567,20.6316872543664,21.606834586676,21.9911485751285),
 .UNSPECIFIED.);
#521=B_SPLINE_CURVE_WITH_KNOTS('',3,(#17356,#17357,#17358,#17359,#17360,
#17361,#17362,#17363,#17364,#17365),.UNSPECIFIED.,.F.,.F.,(4,1,1,1,1,1,
1,4),(15.7079632679489,16.3486947915912,17.3238421239009,18.2989894562105,
19.2741367885202,20.2492841208299,21.2244314531395,21.9911485751285),
 .UNSPECIFIED.);
#522=B_SPLINE_CURVE_WITH_KNOTS('',3,(#17510,#17511,#17512,#17513,#17514,
#17515,#17516,#17517,#17518,#17519,#17520,#17521,#17522,#17523,#17524,#17525,
#17526,#17527,#17528,#17529,#17530,#17531,#17532,#17533,#17534,#17535,#17536,
#17537,#17538,#17539,#17540,#17541,#17542,#17543,#17544,#17545,#17546,#17547,
#17548,#17549,#17550,#17551,#17552,#17553,#17554,#17555,#17556,#17557,#17558),
 .UNSPECIFIED.,.F.,.F.,(4,3,3,3,3,3,3,3,3,3,3,3,3,3,3,3,4),(0.,0.0320333804888866,
0.0505515708593653,0.0603413132804416,0.0917900141854983,0.108096115778005,
0.122914675479851,0.145143248337739,0.168151513577436,0.177516949333476,
0.202471322707608,0.21794283081622,0.231200110368267,0.247503117401854,
0.263651632124391,0.277334442830003,0.286347380332244),.UNSPECIFIED.);
#523=B_SPLINE_CURVE_WITH_KNOTS('',3,(#17559,#17560,#17561,#17562,#17563,
#17564,#17565,#17566,#17567,#17568,#17569,#17570,#17571,#17572,#17573,#17574,
#17575,#17576,#17577,#17578,#17579,#17580,#17581,#17582,#17583,#17584,#17585,
#17586,#17587,#17588,#17589,#17590,#17591,#17592,#17593,#17594,#17595,#17596,
#17597,#17598,#17599,#17600,#17601,#17602,#17603,#17604,#17605,#17606,#17607),
 .UNSPECIFIED.,.F.,.F.,(4,3,3,3,3,3,3,3,3,3,3,3,3,3,3,3,4),(0.,0.0274305464075637,
0.0492901149097146,0.0591933555873536,0.0887250095166089,0.100015570674795,
0.108381796308415,0.130826479038955,0.152531076563578,0.162815893631175,
0.190691958353668,0.212372986031639,0.222945305605857,0.245534254906135,
0.257847836118801,0.274320152521146,0.28514280399515),.UNSPECIFIED.);
#524=B_SPLINE_CURVE_WITH_KNOTS('',3,(#17608,#17609,#17610,#17611,#17612,
#17613,#17614,#17615,#17616,#17617,#17618,#17619,#17620,#17621,#17622,#17623,
#17624,#17625,#17626,#17627,#17628,#17629,#17630,#17631,#17632),
 .UNSPECIFIED.,.F.,.F.,(4,3,3,3,3,3,3,3,4),(-10.1357873115492,-9.75147332309665,
-8.77632599078699,-7.80117865847732,-6.82603132616766,-5.85088399385799,
-4.87573666154833,-3.90058932923866,-3.8526020043696),.UNSPECIFIED.);
#525=B_SPLINE_CURVE_WITH_KNOTS('',3,(#17777,#17778,#17779,#17780,#17781,
#17782,#17783,#17784,#17785,#17786,#17787,#17788,#17789,#17790,#17791,#17792,
#17793,#17794,#17795,#17796,#17797,#17798,#17799,#17800,#17801,#17802,#17803,
#17804,#17805,#17806,#17807,#17808,#17809,#17810,#17811,#17812,#17813,#17814,
#17815,#17816,#17817,#17818,#17819,#17820,#17821,#17822,#17823,#17824,#17825),
 .UNSPECIFIED.,.F.,.F.,(4,3,3,3,3,3,3,3,3,3,3,3,3,3,3,3,4),(0.,0.0274305890506951,
0.0492901290331875,0.0591933603491513,0.0887250177779717,0.100015607166709,
0.108381835831352,0.13082647903896,0.152531071764912,0.162815892251191,
0.190691957318683,0.212372984486691,0.22294529735758,0.245534140364172,
0.257847701250626,0.274320152521159,0.285142803995162),.UNSPECIFIED.);
#526=B_SPLINE_CURVE_WITH_KNOTS('',3,(#17826,#17827,#17828,#17829,#17830,
#17831,#17832,#17833,#17834,#17835,#17836,#17837,#17838,#17839,#17840,#17841,
#17842,#17843,#17844,#17845,#17846,#17847,#17848,#17849,#17850),
 .UNSPECIFIED.,.F.,.F.,(4,3,3,3,3,3,3,3,4),(7.59274844815668,7.80117865847732,
8.77632599078698,9.75147332309665,10.7266206554063,11.701767987716,12.6769153200256,
13.6520626523353,13.8759337553363),.UNSPECIFIED.);
#527=B_SPLINE_CURVE_WITH_KNOTS('',3,(#17851,#17852,#17853,#17854,#17855,
#17856,#17857,#17858,#17859,#17860,#17861,#17862,#17863,#17864,#17865,#17866,
#17867,#17868,#17869,#17870,#17871,#17872,#17873,#17874,#17875,#17876,#17877,
#17878,#17879,#17880,#17881,#17882,#17883,#17884,#17885,#17886,#17887,#17888,
#17889,#17890,#17891,#17892,#17893,#17894,#17895,#17896,#17897,#17898,#17899),
 .UNSPECIFIED.,.F.,.F.,(4,3,3,3,3,3,3,3,3,3,3,3,3,3,3,3,4),(0.,0.0320334058164849,
0.0505515938322513,0.0603413311462071,0.0917900214840119,0.108096111687201,
0.122914678304232,0.145143248337743,0.168151527562726,0.177516955081398,
0.202471327018552,0.217942288122009,0.231200024743484,0.24750284136614,
0.263651600306541,0.277334442830014,0.286347380332252),.UNSPECIFIED.);
#528=B_SPLINE_CURVE_WITH_KNOTS('',3,(#18037,#18038,#18039,#18040,#18041),
 .UNSPECIFIED.,.F.,.F.,(4,1,4),(-0.105712226943305,-0.0453052401185593,
0.),.UNSPECIFIED.);
#529=B_SPLINE_CURVE_WITH_KNOTS('',3,(#18044,#18045,#18046,#18047,#18048),
 .UNSPECIFIED.,.F.,.F.,(4,1,4),(0.,0.0453052401185593,0.105712226943305),
 .UNSPECIFIED.);
#530=B_SPLINE_CURVE_WITH_KNOTS('',3,(#18083,#18084,#18085,#18086,#18087),
 .UNSPECIFIED.,.F.,.F.,(4,1,4),(-0.105712227002476,-0.0453052401439183,
0.),.UNSPECIFIED.);
#531=B_SPLINE_CURVE_WITH_KNOTS('',3,(#18088,#18089,#18090,#18091,#18092),
 .UNSPECIFIED.,.F.,.F.,(4,1,4),(0.,0.0453052401439183,0.105712227002476),
 .UNSPECIFIED.);
#532=B_SPLINE_CURVE_WITH_KNOTS('',3,(#18121,#18122,#18123,#18124,#18125),
 .UNSPECIFIED.,.F.,.F.,(4,1,4),(-9.8118987320379,-4.20509945658767,0.),
 .UNSPECIFIED.);
#533=B_SPLINE_CURVE_WITH_KNOTS('',3,(#18126,#18127,#18128,#18129,#18130),
 .UNSPECIFIED.,.F.,.F.,(4,1,4),(0.,4.20509945658767,9.8118987320379),
 .UNSPECIFIED.);
#534=B_SPLINE_CURVE_WITH_KNOTS('',3,(#18159,#18160,#18161,#18162,#18163),
 .UNSPECIFIED.,.F.,.F.,(4,1,4),(-0.103805833027027,-0.0444882141544403,
0.),.UNSPECIFIED.);
#535=B_SPLINE_CURVE_WITH_KNOTS('',3,(#18164,#18165,#18166,#18167,#18168),
 .UNSPECIFIED.,.F.,.F.,(4,1,4),(0.,0.0444882141544403,0.103805833027027),
 .UNSPECIFIED.);
#536=B_SPLINE_CURVE_WITH_KNOTS('',3,(#18203,#18204,#18205,#18206,#18207),
 .UNSPECIFIED.,.F.,.F.,(4,1,4),(-0.103805833117318,-0.0444882141931362,
-2.06005858395869E-18),.UNSPECIFIED.);
#537=B_SPLINE_CURVE_WITH_KNOTS('',3,(#18208,#18209,#18210,#18211,#18212),
 .UNSPECIFIED.,.F.,.F.,(4,1,4),(2.06005858395869E-18,0.0444882141931362,
0.103805833117318),.UNSPECIFIED.);
#538=B_SPLINE_CURVE_WITH_KNOTS('',3,(#18238,#18239,#18240,#18241,#18242),
 .UNSPECIFIED.,.F.,.F.,(4,1,4),(-9.81189789495051,-4.20509909783593,0.),
 .UNSPECIFIED.);
#539=B_SPLINE_CURVE_WITH_KNOTS('',3,(#18243,#18244,#18245,#18246,#18247),
 .UNSPECIFIED.,.F.,.F.,(4,1,4),(0.,4.20509909783593,9.81189789495051),
 .UNSPECIFIED.);
#540=B_SPLINE_CURVE_WITH_KNOTS('',3,(#18250,#18251,#18252,#18253),
 .UNSPECIFIED.,.F.,.F.,(4,4),(0.00062434729305816,0.125151053668407),
 .UNSPECIFIED.);
#541=B_SPLINE_CURVE_WITH_KNOTS('',3,(#18256,#18257,#18258,#18259),
 .UNSPECIFIED.,.F.,.F.,(4,4),(-0.125151053668407,-0.000624347293058304),
 .UNSPECIFIED.);
#542=B_SPLINE_CURVE_WITH_KNOTS('',3,(#18281,#18282,#18283,#18284),
 .UNSPECIFIED.,.F.,.F.,(4,4),(-0.124859357077656,3.91613824701764E-16),
 .UNSPECIFIED.);
#543=B_SPLINE_CURVE_WITH_KNOTS('',3,(#18285,#18286,#18287,#18288,#18289,
#18290,#18291,#18292,#18293,#18294,#18295,#18296,#18297,#18298,#18299,#18300,
#18301,#18302,#18303,#18304,#18305,#18306,#18307,#18308,#18309,#18310,#18311,
#18312),.UNSPECIFIED.,.F.,.F.,(4,3,3,3,3,3,3,3,3,4),(0.,0.0322709922822142,
0.0586131010579366,0.0908535483049993,0.095660418056781,0.117090121226367,
0.14947943031994,0.17008966569926,0.202270498561131,0.223122165115773),
 .UNSPECIFIED.);
#544=B_SPLINE_CURVE_WITH_KNOTS('',3,(#18330,#18331,#18332,#18333),
 .UNSPECIFIED.,.F.,.F.,(4,4),(1.57426155444895E-16,0.124757292074316),
 .UNSPECIFIED.);
#545=B_SPLINE_CURVE_WITH_KNOTS('',3,(#18334,#18335,#18336,#18337),
 .UNSPECIFIED.,.F.,.F.,(4,4),(0.0135518988075539,0.986045335056425),
 .UNSPECIFIED.);
#546=B_SPLINE_CURVE_WITH_KNOTS('',3,(#18359,#18360,#18361,#18362),
 .UNSPECIFIED.,.F.,.F.,(4,4),(-0.124959300034279,-0.000432357919845506),
 .UNSPECIFIED.);
#547=B_SPLINE_CURVE_WITH_KNOTS('',3,(#18363,#18364,#18365,#18366,#18367,
#18368,#18369,#18370,#18371,#18372,#18373,#18374,#18375,#18376,#18377,#18378,
#18379,#18380,#18381,#18382,#18383,#18384,#18385,#18386,#18387,#18388,#18389,
#18390),.UNSPECIFIED.,.F.,.F.,(4,3,3,3,3,3,3,3,3,4),(0.,0.0322720371751271,
0.0586511315716134,0.0908889384397039,0.0974306796249642,0.117149930269381,
0.149553095257184,0.172178760978465,0.204364325027201,0.227238249760569),
 .UNSPECIFIED.);
#548=B_SPLINE_CURVE_WITH_KNOTS('',3,(#18394,#18395,#18396,#18397),
 .UNSPECIFIED.,.F.,.F.,(4,4),(0.000432357919845864,0.124959300034279),
 .UNSPECIFIED.);
#549=B_SPLINE_CURVE_WITH_KNOTS('',3,(#18420,#18421,#18422,#18423,#18424,
#18425,#18426,#18427,#18428,#18429,#18430,#18431,#18432,#18433,#18434,#18435,
#18436,#18437,#18438,#18439,#18440,#18441,#18442,#18443,#18444,#18445,#18446,
#18447),.UNSPECIFIED.,.F.,.F.,(4,3,3,3,3,3,3,3,3,4),(0.,0.0322770007607458,
0.0586509099358757,0.0908890592373506,0.0956758252683957,0.117149647541228,
0.149540928065794,0.17012301918783,0.202296660223156,0.2231241621482),
 .UNSPECIFIED.);
#550=B_SPLINE_CURVE_WITH_KNOTS('',3,(#18448,#18449,#18450,#18451),
 .UNSPECIFIED.,.F.,.F.,(4,4),(1.94722710178397E-16,0.124859357077656),
 .UNSPECIFIED.);
#551=B_SPLINE_CURVE_WITH_KNOTS('',3,(#18473,#18474,#18475,#18476),
 .UNSPECIFIED.,.F.,.F.,(4,4),(-0.124757292074297,-2.43294967505747E-16),
 .UNSPECIFIED.);
#552=B_SPLINE_CURVE_WITH_KNOTS('',3,(#18477,#18478,#18479,#18480,#18481,
#18482,#18483,#18484,#18485,#18486,#18487,#18488,#18489,#18490,#18491,#18492,
#18493,#18494,#18495,#18496,#18497,#18498,#18499,#18500,#18501,#18502,#18503,
#18504),.UNSPECIFIED.,.F.,.F.,(4,3,3,3,3,3,3,3,3,4),(0.,0.0322677829554273,
0.0586251784806003,0.0908644978360146,0.097419835848357,0.117108565494702,
0.149510109206484,0.172155480916619,0.204345933772221,0.227236831322489),
 .UNSPECIFIED.);
#553=B_SPLINE_CURVE_WITH_KNOTS('',3,(#18506,#18507,#18508,#18509),
 .UNSPECIFIED.,.F.,.F.,(4,4),(0.0139546649435756,0.986448101192446),
 .UNSPECIFIED.);
#554=SHAPE_REPRESENTATION_RELATIONSHIP('SRR','None',#18624,#563);
#555=SHAPE_REPRESENTATION_RELATIONSHIP('SRR','None',#18625,#564);
#556=SHAPE_REPRESENTATION_RELATIONSHIP('SRR','None',#18626,#565);
#557=SHAPE_REPRESENTATION_RELATIONSHIP('SRR','None',#18628,#566);
#558=SHAPE_REPRESENTATION_RELATIONSHIP('SRR','None',#18629,#567);
#559=SHAPE_REPRESENTATION_RELATIONSHIP('SRR','None',#18630,#568);
#560=SHAPE_REPRESENTATION_RELATIONSHIP('SRR','None',#18631,#569);
#561=SHAPE_REPRESENTATION_RELATIONSHIP('SRR','None',#18632,#570);
#562=SHAPE_REPRESENTATION_RELATIONSHIP('SRR','None',#18633,#571);
#563=ADVANCED_BREP_SHAPE_REPRESENTATION('',(#581),#18570);
#564=ADVANCED_BREP_SHAPE_REPRESENTATION('',(#582),#18571);
#565=ADVANCED_BREP_SHAPE_REPRESENTATION('',(#583),#18572);
#566=ADVANCED_BREP_SHAPE_REPRESENTATION('',(#584),#18574);
#567=ADVANCED_BREP_SHAPE_REPRESENTATION('',(#585),#18575);
#568=ADVANCED_BREP_SHAPE_REPRESENTATION('',(#586),#18576);
#569=ADVANCED_BREP_SHAPE_REPRESENTATION('',(#587),#18577);
#570=ADVANCED_BREP_SHAPE_REPRESENTATION('',(#588),#18578);
#571=ADVANCED_BREP_SHAPE_REPRESENTATION('',(#589),#18579);
#572=STYLED_ITEM('',(#18683),#581);
#573=STYLED_ITEM('',(#18684),#582);
#574=STYLED_ITEM('',(#18685),#583);
#575=STYLED_ITEM('',(#18686),#584);
#576=STYLED_ITEM('',(#18686),#585);
#577=STYLED_ITEM('',(#18685),#586);
#578=STYLED_ITEM('',(#18687),#587);
#579=STYLED_ITEM('',(#18688),#588);
#580=STYLED_ITEM('',(#18689),#589);
#581=MANIFOLD_SOLID_BREP('Body1',#6544);
#582=MANIFOLD_SOLID_BREP('Body1',#6545);
#583=MANIFOLD_SOLID_BREP('Body1',#6546);
#584=MANIFOLD_SOLID_BREP('Body1',#6547);
#585=MANIFOLD_SOLID_BREP('Body1',#6548);
#586=MANIFOLD_SOLID_BREP('Body1',#6549);
#587=MANIFOLD_SOLID_BREP('Body1',#6550);
#588=MANIFOLD_SOLID_BREP('Body1',#6551);
#589=MANIFOLD_SOLID_BREP('Body1',#6552);
#590=FACE_BOUND('',#1186,.T.);
#591=FACE_BOUND('',#1187,.T.);
#592=FACE_BOUND('',#1188,.T.);
#593=FACE_BOUND('',#1196,.T.);
#594=FACE_BOUND('',#1197,.T.);
#595=FACE_BOUND('',#1198,.T.);
#596=FACE_BOUND('',#1207,.T.);
#597=FACE_BOUND('',#1209,.T.);
#598=FACE_BOUND('',#1212,.T.);
#599=FACE_BOUND('',#1230,.T.);
#600=FACE_BOUND('',#1231,.T.);
#601=FACE_BOUND('',#1232,.T.);
#602=FACE_BOUND('',#1239,.T.);
#603=FACE_BOUND('',#1242,.T.);
#604=FACE_BOUND('',#1253,.T.);
#605=FACE_BOUND('',#1255,.T.);
#606=FACE_BOUND('',#1267,.T.);
#607=FACE_BOUND('',#1288,.T.);
#608=FACE_BOUND('',#1289,.T.);
#609=FACE_BOUND('',#1290,.T.);
#610=FACE_BOUND('',#1325,.T.);
#611=FACE_BOUND('',#1326,.T.);
#612=FACE_BOUND('',#1327,.T.);
#613=FACE_BOUND('',#1328,.T.);
#614=FACE_BOUND('',#1329,.T.);
#615=FACE_BOUND('',#1330,.T.);
#616=FACE_BOUND('',#1340,.T.);
#617=FACE_BOUND('',#1341,.T.);
#618=FACE_BOUND('',#1342,.T.);
#619=FACE_BOUND('',#1350,.T.);
#620=FACE_BOUND('',#1358,.T.);
#621=FACE_BOUND('',#1373,.T.);
#622=FACE_BOUND('',#1375,.T.);
#623=FACE_BOUND('',#1387,.T.);
#624=FACE_BOUND('',#1408,.T.);
#625=FACE_BOUND('',#1409,.T.);
#626=FACE_BOUND('',#1410,.T.);
#627=FACE_BOUND('',#1445,.T.);
#628=FACE_BOUND('',#1446,.T.);
#629=FACE_BOUND('',#1447,.T.);
#630=FACE_BOUND('',#1448,.T.);
#631=FACE_BOUND('',#1449,.T.);
#632=FACE_BOUND('',#1450,.T.);
#633=FACE_BOUND('',#1526,.T.);
#634=FACE_BOUND('',#1529,.T.);
#635=FACE_BOUND('',#1545,.T.);
#636=FACE_BOUND('',#1554,.T.);
#637=FACE_BOUND('',#1558,.T.);
#638=FACE_BOUND('',#1562,.T.);
#639=FACE_BOUND('',#1566,.T.);
#640=FACE_BOUND('',#1570,.T.);
#641=FACE_BOUND('',#1590,.T.);
#642=FACE_BOUND('',#1591,.T.);
#643=FACE_BOUND('',#1596,.T.);
#644=FACE_BOUND('',#1597,.T.);
#645=FACE_BOUND('',#1598,.T.);
#646=FACE_BOUND('',#1599,.T.);
#647=FACE_BOUND('',#1600,.T.);
#648=FACE_BOUND('',#1601,.T.);
#649=FACE_BOUND('',#1606,.T.);
#650=FACE_BOUND('',#1608,.T.);
#651=PLANE('',#6664);
#652=PLANE('',#6665);
#653=PLANE('',#6666);
#654=PLANE('',#6667);
#655=PLANE('',#6668);
#656=PLANE('',#6669);
#657=PLANE('',#6670);
#658=PLANE('',#6671);
#659=PLANE('',#6672);
#660=PLANE('',#6673);
#661=PLANE('',#6674);
#662=PLANE('',#6677);
#663=PLANE('',#6678);
#664=PLANE('',#6679);
#665=PLANE('',#6680);
#666=PLANE('',#6685);
#667=PLANE('',#6686);
#668=PLANE('',#6687);
#669=PLANE('',#6688);
#670=PLANE('',#6689);
#671=PLANE('',#6690);
#672=PLANE('',#6691);
#673=PLANE('',#6696);
#674=PLANE('',#6698);
#675=PLANE('',#6702);
#676=PLANE('',#6707);
#677=PLANE('',#6709);
#678=PLANE('',#6711);
#679=PLANE('',#6712);
#680=PLANE('',#6713);
#681=PLANE('',#6720);
#682=PLANE('',#6731);
#683=PLANE('',#6748);
#684=PLANE('',#6753);
#685=PLANE('',#6759);
#686=PLANE('',#6760);
#687=PLANE('',#6761);
#688=PLANE('',#6762);
#689=PLANE('',#6763);
#690=PLANE('',#6764);
#691=PLANE('',#6765);
#692=PLANE('',#6766);
#693=PLANE('',#6768);
#694=PLANE('',#6770);
#695=PLANE('',#6771);
#696=PLANE('',#6772);
#697=PLANE('',#6773);
#698=PLANE('',#6774);
#699=PLANE('',#6775);
#700=PLANE('',#6776);
#701=PLANE('',#6777);
#702=PLANE('',#6778);
#703=PLANE('',#6779);
#704=PLANE('',#6780);
#705=PLANE('',#6784);
#706=PLANE('',#6786);
#707=PLANE('',#6787);
#708=PLANE('',#6788);
#709=PLANE('',#6789);
#710=PLANE('',#6790);
#711=PLANE('',#6791);
#712=PLANE('',#6793);
#713=PLANE('',#6810);
#714=PLANE('',#6829);
#715=PLANE('',#6830);
#716=PLANE('',#6831);
#717=PLANE('',#6841);
#718=PLANE('',#6845);
#719=PLANE('',#6846);
#720=PLANE('',#6847);
#721=PLANE('',#6848);
#722=PLANE('',#6849);
#723=PLANE('',#6850);
#724=PLANE('',#6851);
#725=PLANE('',#6853);
#726=PLANE('',#6854);
#727=PLANE('',#6855);
#728=PLANE('',#6856);
#729=PLANE('',#6857);
#730=PLANE('',#6858);
#731=PLANE('',#6859);
#732=PLANE('',#6875);
#733=PLANE('',#6876);
#734=PLANE('',#6877);
#735=PLANE('',#6878);
#736=PLANE('',#6879);
#737=PLANE('',#6880);
#738=PLANE('',#6881);
#739=PLANE('',#6882);
#740=PLANE('',#6884);
#741=PLANE('',#6886);
#742=PLANE('',#6887);
#743=PLANE('',#6888);
#744=PLANE('',#6889);
#745=PLANE('',#6890);
#746=PLANE('',#6891);
#747=PLANE('',#6892);
#748=PLANE('',#6893);
#749=PLANE('',#6894);
#750=PLANE('',#6895);
#751=PLANE('',#6896);
#752=PLANE('',#6900);
#753=PLANE('',#6902);
#754=PLANE('',#6903);
#755=PLANE('',#6904);
#756=PLANE('',#6905);
#757=PLANE('',#6906);
#758=PLANE('',#6907);
#759=PLANE('',#6909);
#760=PLANE('',#6926);
#761=PLANE('',#6945);
#762=PLANE('',#6946);
#763=PLANE('',#6947);
#764=PLANE('',#7017);
#765=PLANE('',#7018);
#766=PLANE('',#7019);
#767=PLANE('',#7020);
#768=PLANE('',#7021);
#769=PLANE('',#7022);
#770=PLANE('',#7023);
#771=PLANE('',#7024);
#772=PLANE('',#7028);
#773=PLANE('',#7029);
#774=PLANE('',#7047);
#775=PLANE('',#7049);
#776=PLANE('',#7050);
#777=PLANE('',#7051);
#778=PLANE('',#7052);
#779=PLANE('',#7053);
#780=PLANE('',#7054);
#781=PLANE('',#7055);
#782=PLANE('',#7063);
#783=PLANE('',#7068);
#784=PLANE('',#7069);
#785=PLANE('',#7074);
#786=PLANE('',#7075);
#787=PLANE('',#7080);
#788=PLANE('',#7081);
#789=PLANE('',#7086);
#790=PLANE('',#7105);
#791=PLANE('',#7106);
#792=PLANE('',#7107);
#793=PLANE('',#7108);
#794=PLANE('',#7124);
#795=PLANE('',#7125);
#796=FACE_OUTER_BOUND('',#1172,.T.);
#797=FACE_OUTER_BOUND('',#1173,.T.);
#798=FACE_OUTER_BOUND('',#1174,.T.);
#799=FACE_OUTER_BOUND('',#1175,.T.);
#800=FACE_OUTER_BOUND('',#1176,.T.);
#801=FACE_OUTER_BOUND('',#1177,.T.);
#802=FACE_OUTER_BOUND('',#1178,.T.);
#803=FACE_OUTER_BOUND('',#1179,.T.);
#804=FACE_OUTER_BOUND('',#1180,.T.);
#805=FACE_OUTER_BOUND('',#1181,.T.);
#806=FACE_OUTER_BOUND('',#1182,.T.);
#807=FACE_OUTER_BOUND('',#1183,.T.);
#808=FACE_OUTER_BOUND('',#1184,.T.);
#809=FACE_OUTER_BOUND('',#1185,.T.);
#810=FACE_OUTER_BOUND('',#1189,.T.);
#811=FACE_OUTER_BOUND('',#1190,.T.);
#812=FACE_OUTER_BOUND('',#1191,.T.);
#813=FACE_OUTER_BOUND('',#1192,.T.);
#814=FACE_OUTER_BOUND('',#1193,.T.);
#815=FACE_OUTER_BOUND('',#1194,.T.);
#816=FACE_OUTER_BOUND('',#1195,.T.);
#817=FACE_OUTER_BOUND('',#1199,.T.);
#818=FACE_OUTER_BOUND('',#1200,.T.);
#819=FACE_OUTER_BOUND('',#1201,.T.);
#820=FACE_OUTER_BOUND('',#1202,.T.);
#821=FACE_OUTER_BOUND('',#1203,.T.);
#822=FACE_OUTER_BOUND('',#1204,.T.);
#823=FACE_OUTER_BOUND('',#1205,.T.);
#824=FACE_OUTER_BOUND('',#1206,.T.);
#825=FACE_OUTER_BOUND('',#1208,.T.);
#826=FACE_OUTER_BOUND('',#1210,.T.);
#827=FACE_OUTER_BOUND('',#1211,.T.);
#828=FACE_OUTER_BOUND('',#1213,.T.);
#829=FACE_OUTER_BOUND('',#1214,.T.);
#830=FACE_OUTER_BOUND('',#1215,.T.);
#831=FACE_OUTER_BOUND('',#1216,.T.);
#832=FACE_OUTER_BOUND('',#1217,.T.);
#833=FACE_OUTER_BOUND('',#1218,.T.);
#834=FACE_OUTER_BOUND('',#1219,.T.);
#835=FACE_OUTER_BOUND('',#1220,.T.);
#836=FACE_OUTER_BOUND('',#1221,.T.);
#837=FACE_OUTER_BOUND('',#1222,.T.);
#838=FACE_OUTER_BOUND('',#1223,.T.);
#839=FACE_OUTER_BOUND('',#1224,.T.);
#840=FACE_OUTER_BOUND('',#1225,.T.);
#841=FACE_OUTER_BOUND('',#1226,.T.);
#842=FACE_OUTER_BOUND('',#1227,.T.);
#843=FACE_OUTER_BOUND('',#1228,.T.);
#844=FACE_OUTER_BOUND('',#1229,.T.);
#845=FACE_OUTER_BOUND('',#1233,.T.);
#846=FACE_OUTER_BOUND('',#1234,.T.);
#847=FACE_OUTER_BOUND('',#1235,.T.);
#848=FACE_OUTER_BOUND('',#1236,.T.);
#849=FACE_OUTER_BOUND('',#1237,.T.);
#850=FACE_OUTER_BOUND('',#1238,.T.);
#851=FACE_OUTER_BOUND('',#1240,.T.);
#852=FACE_OUTER_BOUND('',#1241,.T.);
#853=FACE_OUTER_BOUND('',#1243,.T.);
#854=FACE_OUTER_BOUND('',#1244,.T.);
#855=FACE_OUTER_BOUND('',#1245,.T.);
#856=FACE_OUTER_BOUND('',#1246,.T.);
#857=FACE_OUTER_BOUND('',#1247,.T.);
#858=FACE_OUTER_BOUND('',#1248,.T.);
#859=FACE_OUTER_BOUND('',#1249,.T.);
#860=FACE_OUTER_BOUND('',#1250,.T.);
#861=FACE_OUTER_BOUND('',#1251,.T.);
#862=FACE_OUTER_BOUND('',#1252,.T.);
#863=FACE_OUTER_BOUND('',#1254,.T.);
#864=FACE_OUTER_BOUND('',#1256,.T.);
#865=FACE_OUTER_BOUND('',#1257,.T.);
#866=FACE_OUTER_BOUND('',#1258,.T.);
#867=FACE_OUTER_BOUND('',#1259,.T.);
#868=FACE_OUTER_BOUND('',#1260,.T.);
#869=FACE_OUTER_BOUND('',#1261,.T.);
#870=FACE_OUTER_BOUND('',#1262,.T.);
#871=FACE_OUTER_BOUND('',#1263,.T.);
#872=FACE_OUTER_BOUND('',#1264,.T.);
#873=FACE_OUTER_BOUND('',#1265,.T.);
#874=FACE_OUTER_BOUND('',#1266,.T.);
#875=FACE_OUTER_BOUND('',#1268,.T.);
#876=FACE_OUTER_BOUND('',#1269,.T.);
#877=FACE_OUTER_BOUND('',#1270,.T.);
#878=FACE_OUTER_BOUND('',#1271,.T.);
#879=FACE_OUTER_BOUND('',#1272,.T.);
#880=FACE_OUTER_BOUND('',#1273,.T.);
#881=FACE_OUTER_BOUND('',#1274,.T.);
#882=FACE_OUTER_BOUND('',#1275,.T.);
#883=FACE_OUTER_BOUND('',#1276,.T.);
#884=FACE_OUTER_BOUND('',#1277,.T.);
#885=FACE_OUTER_BOUND('',#1278,.T.);
#886=FACE_OUTER_BOUND('',#1279,.T.);
#887=FACE_OUTER_BOUND('',#1280,.T.);
#888=FACE_OUTER_BOUND('',#1281,.T.);
#889=FACE_OUTER_BOUND('',#1282,.T.);
#890=FACE_OUTER_BOUND('',#1283,.T.);
#891=FACE_OUTER_BOUND('',#1284,.T.);
#892=FACE_OUTER_BOUND('',#1285,.T.);
#893=FACE_OUTER_BOUND('',#1286,.T.);
#894=FACE_OUTER_BOUND('',#1287,.T.);
#895=FACE_OUTER_BOUND('',#1291,.T.);
#896=FACE_OUTER_BOUND('',#1292,.T.);
#897=FACE_OUTER_BOUND('',#1293,.T.);
#898=FACE_OUTER_BOUND('',#1294,.T.);
#899=FACE_OUTER_BOUND('',#1295,.T.);
#900=FACE_OUTER_BOUND('',#1296,.T.);
#901=FACE_OUTER_BOUND('',#1297,.T.);
#902=FACE_OUTER_BOUND('',#1298,.T.);
#903=FACE_OUTER_BOUND('',#1299,.T.);
#904=FACE_OUTER_BOUND('',#1300,.T.);
#905=FACE_OUTER_BOUND('',#1301,.T.);
#906=FACE_OUTER_BOUND('',#1302,.T.);
#907=FACE_OUTER_BOUND('',#1303,.T.);
#908=FACE_OUTER_BOUND('',#1304,.T.);
#909=FACE_OUTER_BOUND('',#1305,.T.);
#910=FACE_OUTER_BOUND('',#1306,.T.);
#911=FACE_OUTER_BOUND('',#1307,.T.);
#912=FACE_OUTER_BOUND('',#1308,.T.);
#913=FACE_OUTER_BOUND('',#1309,.T.);
#914=FACE_OUTER_BOUND('',#1310,.T.);
#915=FACE_OUTER_BOUND('',#1311,.T.);
#916=FACE_OUTER_BOUND('',#1312,.T.);
#917=FACE_OUTER_BOUND('',#1313,.T.);
#918=FACE_OUTER_BOUND('',#1314,.T.);
#919=FACE_OUTER_BOUND('',#1315,.T.);
#920=FACE_OUTER_BOUND('',#1316,.T.);
#921=FACE_OUTER_BOUND('',#1317,.T.);
#922=FACE_OUTER_BOUND('',#1318,.T.);
#923=FACE_OUTER_BOUND('',#1319,.T.);
#924=FACE_OUTER_BOUND('',#1320,.T.);
#925=FACE_OUTER_BOUND('',#1321,.T.);
#926=FACE_OUTER_BOUND('',#1322,.T.);
#927=FACE_OUTER_BOUND('',#1323,.T.);
#928=FACE_OUTER_BOUND('',#1324,.T.);
#929=FACE_OUTER_BOUND('',#1331,.T.);
#930=FACE_OUTER_BOUND('',#1332,.T.);
#931=FACE_OUTER_BOUND('',#1333,.T.);
#932=FACE_OUTER_BOUND('',#1334,.T.);
#933=FACE_OUTER_BOUND('',#1335,.T.);
#934=FACE_OUTER_BOUND('',#1336,.T.);
#935=FACE_OUTER_BOUND('',#1337,.T.);
#936=FACE_OUTER_BOUND('',#1338,.T.);
#937=FACE_OUTER_BOUND('',#1339,.T.);
#938=FACE_OUTER_BOUND('',#1343,.T.);
#939=FACE_OUTER_BOUND('',#1344,.T.);
#940=FACE_OUTER_BOUND('',#1345,.T.);
#941=FACE_OUTER_BOUND('',#1346,.T.);
#942=FACE_OUTER_BOUND('',#1347,.T.);
#943=FACE_OUTER_BOUND('',#1348,.T.);
#944=FACE_OUTER_BOUND('',#1349,.T.);
#945=FACE_OUTER_BOUND('',#1351,.T.);
#946=FACE_OUTER_BOUND('',#1352,.T.);
#947=FACE_OUTER_BOUND('',#1353,.T.);
#948=FACE_OUTER_BOUND('',#1354,.T.);
#949=FACE_OUTER_BOUND('',#1355,.T.);
#950=FACE_OUTER_BOUND('',#1356,.T.);
#951=FACE_OUTER_BOUND('',#1357,.T.);
#952=FACE_OUTER_BOUND('',#1359,.T.);
#953=FACE_OUTER_BOUND('',#1360,.T.);
#954=FACE_OUTER_BOUND('',#1361,.T.);
#955=FACE_OUTER_BOUND('',#1362,.T.);
#956=FACE_OUTER_BOUND('',#1363,.T.);
#957=FACE_OUTER_BOUND('',#1364,.T.);
#958=FACE_OUTER_BOUND('',#1365,.T.);
#959=FACE_OUTER_BOUND('',#1366,.T.);
#960=FACE_OUTER_BOUND('',#1367,.T.);
#961=FACE_OUTER_BOUND('',#1368,.T.);
#962=FACE_OUTER_BOUND('',#1369,.T.);
#963=FACE_OUTER_BOUND('',#1370,.T.);
#964=FACE_OUTER_BOUND('',#1371,.T.);
#965=FACE_OUTER_BOUND('',#1372,.T.);
#966=FACE_OUTER_BOUND('',#1374,.T.);
#967=FACE_OUTER_BOUND('',#1376,.T.);
#968=FACE_OUTER_BOUND('',#1377,.T.);
#969=FACE_OUTER_BOUND('',#1378,.T.);
#970=FACE_OUTER_BOUND('',#1379,.T.);
#971=FACE_OUTER_BOUND('',#1380,.T.);
#972=FACE_OUTER_BOUND('',#1381,.T.);
#973=FACE_OUTER_BOUND('',#1382,.T.);
#974=FACE_OUTER_BOUND('',#1383,.T.);
#975=FACE_OUTER_BOUND('',#1384,.T.);
#976=FACE_OUTER_BOUND('',#1385,.T.);
#977=FACE_OUTER_BOUND('',#1386,.T.);
#978=FACE_OUTER_BOUND('',#1388,.T.);
#979=FACE_OUTER_BOUND('',#1389,.T.);
#980=FACE_OUTER_BOUND('',#1390,.T.);
#981=FACE_OUTER_BOUND('',#1391,.T.);
#982=FACE_OUTER_BOUND('',#1392,.T.);
#983=FACE_OUTER_BOUND('',#1393,.T.);
#984=FACE_OUTER_BOUND('',#1394,.T.);
#985=FACE_OUTER_BOUND('',#1395,.T.);
#986=FACE_OUTER_BOUND('',#1396,.T.);
#987=FACE_OUTER_BOUND('',#1397,.T.);
#988=FACE_OUTER_BOUND('',#1398,.T.);
#989=FACE_OUTER_BOUND('',#1399,.T.);
#990=FACE_OUTER_BOUND('',#1400,.T.);
#991=FACE_OUTER_BOUND('',#1401,.T.);
#992=FACE_OUTER_BOUND('',#1402,.T.);
#993=FACE_OUTER_BOUND('',#1403,.T.);
#994=FACE_OUTER_BOUND('',#1404,.T.);
#995=FACE_OUTER_BOUND('',#1405,.T.);
#996=FACE_OUTER_BOUND('',#1406,.T.);
#997=FACE_OUTER_BOUND('',#1407,.T.);
#998=FACE_OUTER_BOUND('',#1411,.T.);
#999=FACE_OUTER_BOUND('',#1412,.T.);
#1000=FACE_OUTER_BOUND('',#1413,.T.);
#1001=FACE_OUTER_BOUND('',#1414,.T.);
#1002=FACE_OUTER_BOUND('',#1415,.T.);
#1003=FACE_OUTER_BOUND('',#1416,.T.);
#1004=FACE_OUTER_BOUND('',#1417,.T.);
#1005=FACE_OUTER_BOUND('',#1418,.T.);
#1006=FACE_OUTER_BOUND('',#1419,.T.);
#1007=FACE_OUTER_BOUND('',#1420,.T.);
#1008=FACE_OUTER_BOUND('',#1421,.T.);
#1009=FACE_OUTER_BOUND('',#1422,.T.);
#1010=FACE_OUTER_BOUND('',#1423,.T.);
#1011=FACE_OUTER_BOUND('',#1424,.T.);
#1012=FACE_OUTER_BOUND('',#1425,.T.);
#1013=FACE_OUTER_BOUND('',#1426,.T.);
#1014=FACE_OUTER_BOUND('',#1427,.T.);
#1015=FACE_OUTER_BOUND('',#1428,.T.);
#1016=FACE_OUTER_BOUND('',#1429,.T.);
#1017=FACE_OUTER_BOUND('',#1430,.T.);
#1018=FACE_OUTER_BOUND('',#1431,.T.);
#1019=FACE_OUTER_BOUND('',#1432,.T.);
#1020=FACE_OUTER_BOUND('',#1433,.T.);
#1021=FACE_OUTER_BOUND('',#1434,.T.);
#1022=FACE_OUTER_BOUND('',#1435,.T.);
#1023=FACE_OUTER_BOUND('',#1436,.T.);
#1024=FACE_OUTER_BOUND('',#1437,.T.);
#1025=FACE_OUTER_BOUND('',#1438,.T.);
#1026=FACE_OUTER_BOUND('',#1439,.T.);
#1027=FACE_OUTER_BOUND('',#1440,.T.);
#1028=FACE_OUTER_BOUND('',#1441,.T.);
#1029=FACE_OUTER_BOUND('',#1442,.T.);
#1030=FACE_OUTER_BOUND('',#1443,.T.);
#1031=FACE_OUTER_BOUND('',#1444,.T.);
#1032=FACE_OUTER_BOUND('',#1451,.T.);
#1033=FACE_OUTER_BOUND('',#1452,.T.);
#1034=FACE_OUTER_BOUND('',#1453,.T.);
#1035=FACE_OUTER_BOUND('',#1454,.T.);
#1036=FACE_OUTER_BOUND('',#1455,.T.);
#1037=FACE_OUTER_BOUND('',#1456,.T.);
#1038=FACE_OUTER_BOUND('',#1457,.T.);
#1039=FACE_OUTER_BOUND('',#1458,.T.);
#1040=FACE_OUTER_BOUND('',#1459,.T.);
#1041=FACE_OUTER_BOUND('',#1460,.T.);
#1042=FACE_OUTER_BOUND('',#1461,.T.);
#1043=FACE_OUTER_BOUND('',#1462,.T.);
#1044=FACE_OUTER_BOUND('',#1463,.T.);
#1045=FACE_OUTER_BOUND('',#1464,.T.);
#1046=FACE_OUTER_BOUND('',#1465,.T.);
#1047=FACE_OUTER_BOUND('',#1466,.T.);
#1048=FACE_OUTER_BOUND('',#1467,.T.);
#1049=FACE_OUTER_BOUND('',#1468,.T.);
#1050=FACE_OUTER_BOUND('',#1469,.T.);
#1051=FACE_OUTER_BOUND('',#1470,.T.);
#1052=FACE_OUTER_BOUND('',#1471,.T.);
#1053=FACE_OUTER_BOUND('',#1472,.T.);
#1054=FACE_OUTER_BOUND('',#1473,.T.);
#1055=FACE_OUTER_BOUND('',#1474,.T.);
#1056=FACE_OUTER_BOUND('',#1475,.T.);
#1057=FACE_OUTER_BOUND('',#1476,.T.);
#1058=FACE_OUTER_BOUND('',#1477,.T.);
#1059=FACE_OUTER_BOUND('',#1478,.T.);
#1060=FACE_OUTER_BOUND('',#1479,.T.);
#1061=FACE_OUTER_BOUND('',#1480,.T.);
#1062=FACE_OUTER_BOUND('',#1481,.T.);
#1063=FACE_OUTER_BOUND('',#1482,.T.);
#1064=FACE_OUTER_BOUND('',#1483,.T.);
#1065=FACE_OUTER_BOUND('',#1484,.T.);
#1066=FACE_OUTER_BOUND('',#1485,.T.);
#1067=FACE_OUTER_BOUND('',#1486,.T.);
#1068=FACE_OUTER_BOUND('',#1487,.T.);
#1069=FACE_OUTER_BOUND('',#1488,.T.);
#1070=FACE_OUTER_BOUND('',#1489,.T.);
#1071=FACE_OUTER_BOUND('',#1490,.T.);
#1072=FACE_OUTER_BOUND('',#1491,.T.);
#1073=FACE_OUTER_BOUND('',#1492,.T.);
#1074=FACE_OUTER_BOUND('',#1493,.T.);
#1075=FACE_OUTER_BOUND('',#1494,.T.);
#1076=FACE_OUTER_BOUND('',#1495,.T.);
#1077=FACE_OUTER_BOUND('',#1496,.T.);
#1078=FACE_OUTER_BOUND('',#1497,.T.);
#1079=FACE_OUTER_BOUND('',#1498,.T.);
#1080=FACE_OUTER_BOUND('',#1499,.T.);
#1081=FACE_OUTER_BOUND('',#1500,.T.);
#1082=FACE_OUTER_BOUND('',#1501,.T.);
#1083=FACE_OUTER_BOUND('',#1502,.T.);
#1084=FACE_OUTER_BOUND('',#1503,.T.);
#1085=FACE_OUTER_BOUND('',#1504,.T.);
#1086=FACE_OUTER_BOUND('',#1505,.T.);
#1087=FACE_OUTER_BOUND('',#1506,.T.);
#1088=FACE_OUTER_BOUND('',#1507,.T.);
#1089=FACE_OUTER_BOUND('',#1508,.T.);
#1090=FACE_OUTER_BOUND('',#1509,.T.);
#1091=FACE_OUTER_BOUND('',#1510,.T.);
#1092=FACE_OUTER_BOUND('',#1511,.T.);
#1093=FACE_OUTER_BOUND('',#1512,.T.);
#1094=FACE_OUTER_BOUND('',#1513,.T.);
#1095=FACE_OUTER_BOUND('',#1514,.T.);
#1096=FACE_OUTER_BOUND('',#1515,.T.);
#1097=FACE_OUTER_BOUND('',#1516,.T.);
#1098=FACE_OUTER_BOUND('',#1517,.T.);
#1099=FACE_OUTER_BOUND('',#1518,.T.);
#1100=FACE_OUTER_BOUND('',#1519,.T.);
#1101=FACE_OUTER_BOUND('',#1520,.T.);
#1102=FACE_OUTER_BOUND('',#1521,.T.);
#1103=FACE_OUTER_BOUND('',#1522,.T.);
#1104=FACE_OUTER_BOUND('',#1523,.T.);
#1105=FACE_OUTER_BOUND('',#1524,.T.);
#1106=FACE_OUTER_BOUND('',#1525,.T.);
#1107=FACE_OUTER_BOUND('',#1527,.T.);
#1108=FACE_OUTER_BOUND('',#1528,.T.);
#1109=FACE_OUTER_BOUND('',#1530,.T.);
#1110=FACE_OUTER_BOUND('',#1531,.T.);
#1111=FACE_OUTER_BOUND('',#1532,.T.);
#1112=FACE_OUTER_BOUND('',#1533,.T.);
#1113=FACE_OUTER_BOUND('',#1534,.T.);
#1114=FACE_OUTER_BOUND('',#1535,.T.);
#1115=FACE_OUTER_BOUND('',#1536,.T.);
#1116=FACE_OUTER_BOUND('',#1537,.T.);
#1117=FACE_OUTER_BOUND('',#1538,.T.);
#1118=FACE_OUTER_BOUND('',#1539,.T.);
#1119=FACE_OUTER_BOUND('',#1540,.T.);
#1120=FACE_OUTER_BOUND('',#1541,.T.);
#1121=FACE_OUTER_BOUND('',#1542,.T.);
#1122=FACE_OUTER_BOUND('',#1543,.T.);
#1123=FACE_OUTER_BOUND('',#1544,.T.);
#1124=FACE_OUTER_BOUND('',#1546,.T.);
#1125=FACE_OUTER_BOUND('',#1547,.T.);
#1126=FACE_OUTER_BOUND('',#1548,.T.);
#1127=FACE_OUTER_BOUND('',#1549,.T.);
#1128=FACE_OUTER_BOUND('',#1550,.T.);
#1129=FACE_OUTER_BOUND('',#1551,.T.);
#1130=FACE_OUTER_BOUND('',#1552,.T.);
#1131=FACE_OUTER_BOUND('',#1553,.T.);
#1132=FACE_OUTER_BOUND('',#1555,.T.);
#1133=FACE_OUTER_BOUND('',#1556,.T.);
#1134=FACE_OUTER_BOUND('',#1557,.T.);
#1135=FACE_OUTER_BOUND('',#1559,.T.);
#1136=FACE_OUTER_BOUND('',#1560,.T.);
#1137=FACE_OUTER_BOUND('',#1561,.T.);
#1138=FACE_OUTER_BOUND('',#1563,.T.);
#1139=FACE_OUTER_BOUND('',#1564,.T.);
#1140=FACE_OUTER_BOUND('',#1565,.T.);
#1141=FACE_OUTER_BOUND('',#1567,.T.);
#1142=FACE_OUTER_BOUND('',#1568,.T.);
#1143=FACE_OUTER_BOUND('',#1569,.T.);
#1144=FACE_OUTER_BOUND('',#1571,.T.);
#1145=FACE_OUTER_BOUND('',#1572,.T.);
#1146=FACE_OUTER_BOUND('',#1573,.T.);
#1147=FACE_OUTER_BOUND('',#1574,.T.);
#1148=FACE_OUTER_BOUND('',#1575,.T.);
#1149=FACE_OUTER_BOUND('',#1576,.T.);
#1150=FACE_OUTER_BOUND('',#1577,.T.);
#1151=FACE_OUTER_BOUND('',#1578,.T.);
#1152=FACE_OUTER_BOUND('',#1579,.T.);
#1153=FACE_OUTER_BOUND('',#1580,.T.);
#1154=FACE_OUTER_BOUND('',#1581,.T.);
#1155=FACE_OUTER_BOUND('',#1582,.T.);
#1156=FACE_OUTER_BOUND('',#1583,.T.);
#1157=FACE_OUTER_BOUND('',#1584,.T.);
#1158=FACE_OUTER_BOUND('',#1585,.T.);
#1159=FACE_OUTER_BOUND('',#1586,.T.);
#1160=FACE_OUTER_BOUND('',#1587,.T.);
#1161=FACE_OUTER_BOUND('',#1588,.T.);
#1162=FACE_OUTER_BOUND('',#1589,.T.);
#1163=FACE_OUTER_BOUND('',#1592,.T.);
#1164=FACE_OUTER_BOUND('',#1593,.T.);
#1165=FACE_OUTER_BOUND('',#1594,.T.);
#1166=FACE_OUTER_BOUND('',#1595,.T.);
#1167=FACE_OUTER_BOUND('',#1602,.T.);
#1168=FACE_OUTER_BOUND('',#1603,.T.);
#1169=FACE_OUTER_BOUND('',#1604,.T.);
#1170=FACE_OUTER_BOUND('',#1605,.T.);
#1171=FACE_OUTER_BOUND('',#1607,.T.);
#1172=EDGE_LOOP('',(#4140,#4141,#4142,#4143));
#1173=EDGE_LOOP('',(#4144,#4145,#4146,#4147));
#1174=EDGE_LOOP('',(#4148,#4149,#4150,#4151));
#1175=EDGE_LOOP('',(#4152,#4153,#4154));
#1176=EDGE_LOOP('',(#4155,#4156,#4157,#4158,#4159));
#1177=EDGE_LOOP('',(#4160,#4161,#4162,#4163));
#1178=EDGE_LOOP('',(#4164,#4165,#4166));
#1179=EDGE_LOOP('',(#4167,#4168,#4169,#4170,#4171,#4172,#4173));
#1180=EDGE_LOOP('',(#4174,#4175,#4176,#4177));
#1181=EDGE_LOOP('',(#4178,#4179,#4180,#4181));
#1182=EDGE_LOOP('',(#4182,#4183,#4184,#4185));
#1183=EDGE_LOOP('',(#4186,#4187,#4188,#4189,#4190,#4191,#4192));
#1184=EDGE_LOOP('',(#4193,#4194,#4195,#4196));
#1185=EDGE_LOOP('',(#4197,#4198,#4199,#4200,#4201,#4202,#4203,#4204,#4205,
#4206,#4207,#4208,#4209,#4210,#4211,#4212,#4213,#4214,#4215));
#1186=EDGE_LOOP('',(#4216));
#1187=EDGE_LOOP('',(#4217));
#1188=EDGE_LOOP('',(#4218));
#1189=EDGE_LOOP('',(#4219,#4220,#4221,#4222));
#1190=EDGE_LOOP('',(#4223,#4224,#4225,#4226,#4227,#4228,#4229,#4230));
#1191=EDGE_LOOP('',(#4231,#4232,#4233,#4234));
#1192=EDGE_LOOP('',(#4235,#4236,#4237,#4238));
#1193=EDGE_LOOP('',(#4239,#4240,#4241,#4242));
#1194=EDGE_LOOP('',(#4243,#4244,#4245,#4246));
#1195=EDGE_LOOP('',(#4247,#4248,#4249,#4250,#4251,#4252,#4253,#4254,#4255,
#4256,#4257,#4258));
#1196=EDGE_LOOP('',(#4259));
#1197=EDGE_LOOP('',(#4260));
#1198=EDGE_LOOP('',(#4261));
#1199=EDGE_LOOP('',(#4262,#4263,#4264,#4265));
#1200=EDGE_LOOP('',(#4266,#4267,#4268,#4269));
#1201=EDGE_LOOP('',(#4270,#4271,#4272,#4273));
#1202=EDGE_LOOP('',(#4274,#4275,#4276,#4277));
#1203=EDGE_LOOP('',(#4278,#4279,#4280,#4281));
#1204=EDGE_LOOP('',(#4282,#4283,#4284,#4285));
#1205=EDGE_LOOP('',(#4286,#4287,#4288,#4289));
#1206=EDGE_LOOP('',(#4290));
#1207=EDGE_LOOP('',(#4291));
#1208=EDGE_LOOP('',(#4292));
#1209=EDGE_LOOP('',(#4293));
#1210=EDGE_LOOP('',(#4294,#4295,#4296,#4297));
#1211=EDGE_LOOP('',(#4298));
#1212=EDGE_LOOP('',(#4299));
#1213=EDGE_LOOP('',(#4300,#4301,#4302,#4303));
#1214=EDGE_LOOP('',(#4304));
#1215=EDGE_LOOP('',(#4305,#4306,#4307,#4308));
#1216=EDGE_LOOP('',(#4309));
#1217=EDGE_LOOP('',(#4310,#4311,#4312,#4313));
#1218=EDGE_LOOP('',(#4314,#4315,#4316,#4317));
#1219=EDGE_LOOP('',(#4318,#4319,#4320,#4321));
#1220=EDGE_LOOP('',(#4322,#4323,#4324,#4325));
#1221=EDGE_LOOP('',(#4326,#4327,#4328,#4329));
#1222=EDGE_LOOP('',(#4330,#4331,#4332,#4333));
#1223=EDGE_LOOP('',(#4334,#4335));
#1224=EDGE_LOOP('',(#4336,#4337));
#1225=EDGE_LOOP('',(#4338,#4339));
#1226=EDGE_LOOP('',(#4340,#4341));
#1227=EDGE_LOOP('',(#4342,#4343,#4344,#4345,#4346,#4347));
#1228=EDGE_LOOP('',(#4348,#4349,#4350,#4351,#4352,#4353));
#1229=EDGE_LOOP('',(#4354,#4355,#4356,#4357,#4358,#4359,#4360,#4361));
#1230=EDGE_LOOP('',(#4362));
#1231=EDGE_LOOP('',(#4363));
#1232=EDGE_LOOP('',(#4364));
#1233=EDGE_LOOP('',(#4365,#4366,#4367,#4368));
#1234=EDGE_LOOP('',(#4369,#4370,#4371,#4372));
#1235=EDGE_LOOP('',(#4373,#4374,#4375,#4376));
#1236=EDGE_LOOP('',(#4377,#4378,#4379,#4380));
#1237=EDGE_LOOP('',(#4381,#4382,#4383,#4384));
#1238=EDGE_LOOP('',(#4385));
#1239=EDGE_LOOP('',(#4386));
#1240=EDGE_LOOP('',(#4387,#4388,#4389,#4390));
#1241=EDGE_LOOP('',(#4391));
#1242=EDGE_LOOP('',(#4392));
#1243=EDGE_LOOP('',(#4393,#4394,#4395,#4396));
#1244=EDGE_LOOP('',(#4397,#4398,#4399,#4400));
#1245=EDGE_LOOP('',(#4401,#4402,#4403,#4404));
#1246=EDGE_LOOP('',(#4405,#4406,#4407,#4408));
#1247=EDGE_LOOP('',(#4409,#4410,#4411,#4412));
#1248=EDGE_LOOP('',(#4413,#4414,#4415,#4416));
#1249=EDGE_LOOP('',(#4417,#4418,#4419,#4420));
#1250=EDGE_LOOP('',(#4421,#4422,#4423,#4424));
#1251=EDGE_LOOP('',(#4425,#4426,#4427,#4428));
#1252=EDGE_LOOP('',(#4429));
#1253=EDGE_LOOP('',(#4430));
#1254=EDGE_LOOP('',(#4431));
#1255=EDGE_LOOP('',(#4432));
#1256=EDGE_LOOP('',(#4433,#4434,#4435,#4436));
#1257=EDGE_LOOP('',(#4437,#4438,#4439,#4440));
#1258=EDGE_LOOP('',(#4441,#4442,#4443,#4444));
#1259=EDGE_LOOP('',(#4445,#4446,#4447,#4448));
#1260=EDGE_LOOP('',(#4449,#4450,#4451,#4452));
#1261=EDGE_LOOP('',(#4453,#4454,#4455,#4456,#4457,#4458));
#1262=EDGE_LOOP('',(#4459,#4460,#4461,#4462,#4463,#4464,#4465,#4466,#4467,
#4468));
#1263=EDGE_LOOP('',(#4469,#4470,#4471,#4472,#4473,#4474,#4475,#4476,#4477,
#4478));
#1264=EDGE_LOOP('',(#4479,#4480,#4481,#4482,#4483,#4484,#4485,#4486,#4487,
#4488));
#1265=EDGE_LOOP('',(#4489,#4490,#4491,#4492,#4493,#4494,#4495,#4496));
#1266=EDGE_LOOP('',(#4497,#4498,#4499,#4500,#4501,#4502,#4503,#4504,#4505,
#4506,#4507,#4508,#4509,#4510,#4511,#4512,#4513,#4514,#4515,#4516,#4517,
#4518,#4519,#4520,#4521,#4522,#4523,#4524,#4525,#4526,#4527,#4528,#4529,
#4530,#4531,#4532,#4533,#4534,#4535,#4536,#4537,#4538));
#1267=EDGE_LOOP('',(#4539,#4540,#4541,#4542,#4543,#4544));
#1268=EDGE_LOOP('',(#4545,#4546,#4547,#4548));
#1269=EDGE_LOOP('',(#4549,#4550,#4551,#4552));
#1270=EDGE_LOOP('',(#4553,#4554,#4555,#4556,#4557,#4558));
#1271=EDGE_LOOP('',(#4559,#4560,#4561,#4562));
#1272=EDGE_LOOP('',(#4563,#4564,#4565,#4566));
#1273=EDGE_LOOP('',(#4567,#4568,#4569,#4570,#4571,#4572));
#1274=EDGE_LOOP('',(#4573,#4574,#4575,#4576));
#1275=EDGE_LOOP('',(#4577,#4578,#4579,#4580));
#1276=EDGE_LOOP('',(#4581,#4582,#4583,#4584));
#1277=EDGE_LOOP('',(#4585,#4586,#4587,#4588));
#1278=EDGE_LOOP('',(#4589,#4590,#4591,#4592,#4593,#4594,#4595,#4596,#4597,
#4598));
#1279=EDGE_LOOP('',(#4599,#4600,#4601,#4602));
#1280=EDGE_LOOP('',(#4603,#4604,#4605,#4606));
#1281=EDGE_LOOP('',(#4607,#4608,#4609,#4610));
#1282=EDGE_LOOP('',(#4611,#4612,#4613,#4614));
#1283=EDGE_LOOP('',(#4615,#4616,#4617,#4618));
#1284=EDGE_LOOP('',(#4619,#4620,#4621,#4622,#4623,#4624,#4625,#4626,#4627,
#4628));
#1285=EDGE_LOOP('',(#4629,#4630,#4631,#4632));
#1286=EDGE_LOOP('',(#4633,#4634,#4635,#4636,#4637,#4638));
#1287=EDGE_LOOP('',(#4639,#4640,#4641,#4642,#4643,#4644,#4645,#4646));
#1288=EDGE_LOOP('',(#4647));
#1289=EDGE_LOOP('',(#4648));
#1290=EDGE_LOOP('',(#4649));
#1291=EDGE_LOOP('',(#4650,#4651,#4652,#4653));
#1292=EDGE_LOOP('',(#4654,#4655,#4656,#4657,#4658,#4659,#4660,#4661,#4662,
#4663));
#1293=EDGE_LOOP('',(#4664,#4665,#4666,#4667));
#1294=EDGE_LOOP('',(#4668,#4669,#4670,#4671));
#1295=EDGE_LOOP('',(#4672,#4673,#4674,#4675));
#1296=EDGE_LOOP('',(#4676,#4677,#4678,#4679));
#1297=EDGE_LOOP('',(#4680,#4681,#4682,#4683));
#1298=EDGE_LOOP('',(#4684,#4685,#4686));
#1299=EDGE_LOOP('',(#4687,#4688,#4689));
#1300=EDGE_LOOP('',(#4690,#4691,#4692));
#1301=EDGE_LOOP('',(#4693,#4694,#4695,#4696));
#1302=EDGE_LOOP('',(#4697,#4698,#4699,#4700));
#1303=EDGE_LOOP('',(#4701,#4702,#4703));
#1304=EDGE_LOOP('',(#4704,#4705,#4706,#4707));
#1305=EDGE_LOOP('',(#4708,#4709,#4710,#4711));
#1306=EDGE_LOOP('',(#4712,#4713,#4714,#4715));
#1307=EDGE_LOOP('',(#4716,#4717,#4718,#4719));
#1308=EDGE_LOOP('',(#4720,#4721,#4722,#4723));
#1309=EDGE_LOOP('',(#4724,#4725,#4726,#4727));
#1310=EDGE_LOOP('',(#4728,#4729,#4730));
#1311=EDGE_LOOP('',(#4731,#4732,#4733));
#1312=EDGE_LOOP('',(#4734,#4735,#4736));
#1313=EDGE_LOOP('',(#4737,#4738,#4739,#4740));
#1314=EDGE_LOOP('',(#4741,#4742,#4743,#4744));
#1315=EDGE_LOOP('',(#4745,#4746,#4747));
#1316=EDGE_LOOP('',(#4748,#4749,#4750,#4751));
#1317=EDGE_LOOP('',(#4752,#4753,#4754,#4755));
#1318=EDGE_LOOP('',(#4756,#4757,#4758,#4759));
#1319=EDGE_LOOP('',(#4760,#4761,#4762,#4763));
#1320=EDGE_LOOP('',(#4764,#4765,#4766,#4767));
#1321=EDGE_LOOP('',(#4768,#4769,#4770,#4771));
#1322=EDGE_LOOP('',(#4772,#4773,#4774,#4775));
#1323=EDGE_LOOP('',(#4776,#4777,#4778,#4779,#4780,#4781,#4782,#4783));
#1324=EDGE_LOOP('',(#4784,#4785,#4786,#4787));
#1325=EDGE_LOOP('',(#4788));
#1326=EDGE_LOOP('',(#4789));
#1327=EDGE_LOOP('',(#4790));
#1328=EDGE_LOOP('',(#4791));
#1329=EDGE_LOOP('',(#4792));
#1330=EDGE_LOOP('',(#4793));
#1331=EDGE_LOOP('',(#4794,#4795,#4796,#4797));
#1332=EDGE_LOOP('',(#4798,#4799,#4800,#4801));
#1333=EDGE_LOOP('',(#4802,#4803));
#1334=EDGE_LOOP('',(#4804,#4805));
#1335=EDGE_LOOP('',(#4806,#4807));
#1336=EDGE_LOOP('',(#4808,#4809));
#1337=EDGE_LOOP('',(#4810,#4811,#4812,#4813,#4814,#4815));
#1338=EDGE_LOOP('',(#4816,#4817,#4818,#4819,#4820,#4821));
#1339=EDGE_LOOP('',(#4822,#4823,#4824,#4825,#4826,#4827,#4828,#4829));
#1340=EDGE_LOOP('',(#4830));
#1341=EDGE_LOOP('',(#4831));
#1342=EDGE_LOOP('',(#4832));
#1343=EDGE_LOOP('',(#4833,#4834,#4835,#4836));
#1344=EDGE_LOOP('',(#4837,#4838,#4839,#4840));
#1345=EDGE_LOOP('',(#4841,#4842,#4843,#4844));
#1346=EDGE_LOOP('',(#4845,#4846,#4847,#4848));
#1347=EDGE_LOOP('',(#4849,#4850,#4851,#4852));
#1348=EDGE_LOOP('',(#4853,#4854,#4855,#4856));
#1349=EDGE_LOOP('',(#4857,#4858,#4859,#4860,#4861,#4862));
#1350=EDGE_LOOP('',(#4863));
#1351=EDGE_LOOP('',(#4864,#4865,#4866,#4867));
#1352=EDGE_LOOP('',(#4868,#4869,#4870,#4871));
#1353=EDGE_LOOP('',(#4872,#4873,#4874,#4875));
#1354=EDGE_LOOP('',(#4876,#4877,#4878,#4879));
#1355=EDGE_LOOP('',(#4880,#4881,#4882,#4883));
#1356=EDGE_LOOP('',(#4884,#4885,#4886,#4887));
#1357=EDGE_LOOP('',(#4888,#4889,#4890,#4891,#4892,#4893));
#1358=EDGE_LOOP('',(#4894));
#1359=EDGE_LOOP('',(#4895,#4896,#4897,#4898));
#1360=EDGE_LOOP('',(#4899,#4900,#4901,#4902));
#1361=EDGE_LOOP('',(#4903,#4904,#4905,#4906));
#1362=EDGE_LOOP('',(#4907,#4908,#4909,#4910));
#1363=EDGE_LOOP('',(#4911,#4912,#4913,#4914));
#1364=EDGE_LOOP('',(#4915,#4916,#4917,#4918));
#1365=EDGE_LOOP('',(#4919,#4920,#4921,#4922));
#1366=EDGE_LOOP('',(#4923,#4924,#4925,#4926));
#1367=EDGE_LOOP('',(#4927,#4928,#4929,#4930));
#1368=EDGE_LOOP('',(#4931,#4932,#4933,#4934));
#1369=EDGE_LOOP('',(#4935,#4936,#4937,#4938));
#1370=EDGE_LOOP('',(#4939,#4940,#4941,#4942));
#1371=EDGE_LOOP('',(#4943,#4944,#4945,#4946));
#1372=EDGE_LOOP('',(#4947));
#1373=EDGE_LOOP('',(#4948));
#1374=EDGE_LOOP('',(#4949));
#1375=EDGE_LOOP('',(#4950));
#1376=EDGE_LOOP('',(#4951,#4952,#4953,#4954));
#1377=EDGE_LOOP('',(#4955,#4956,#4957,#4958));
#1378=EDGE_LOOP('',(#4959,#4960,#4961,#4962));
#1379=EDGE_LOOP('',(#4963,#4964,#4965,#4966));
#1380=EDGE_LOOP('',(#4967,#4968,#4969,#4970));
#1381=EDGE_LOOP('',(#4971,#4972,#4973,#4974,#4975,#4976));
#1382=EDGE_LOOP('',(#4977,#4978,#4979,#4980,#4981,#4982,#4983,#4984,#4985,
#4986));
#1383=EDGE_LOOP('',(#4987,#4988,#4989,#4990,#4991,#4992,#4993,#4994,#4995,
#4996));
#1384=EDGE_LOOP('',(#4997,#4998,#4999,#5000,#5001,#5002,#5003,#5004,#5005,
#5006));
#1385=EDGE_LOOP('',(#5007,#5008,#5009,#5010,#5011,#5012,#5013,#5014));
#1386=EDGE_LOOP('',(#5015,#5016,#5017,#5018,#5019,#5020,#5021,#5022,#5023,
#5024,#5025,#5026,#5027,#5028,#5029,#5030,#5031,#5032,#5033,#5034,#5035,
#5036,#5037,#5038,#5039,#5040,#5041,#5042,#5043,#5044,#5045,#5046,#5047,
#5048,#5049,#5050,#5051,#5052,#5053,#5054,#5055,#5056));
#1387=EDGE_LOOP('',(#5057,#5058,#5059,#5060,#5061,#5062));
#1388=EDGE_LOOP('',(#5063,#5064,#5065,#5066));
#1389=EDGE_LOOP('',(#5067,#5068,#5069,#5070));
#1390=EDGE_LOOP('',(#5071,#5072,#5073,#5074,#5075,#5076));
#1391=EDGE_LOOP('',(#5077,#5078,#5079,#5080));
#1392=EDGE_LOOP('',(#5081,#5082,#5083,#5084));
#1393=EDGE_LOOP('',(#5085,#5086,#5087,#5088,#5089,#5090));
#1394=EDGE_LOOP('',(#5091,#5092,#5093,#5094));
#1395=EDGE_LOOP('',(#5095,#5096,#5097,#5098));
#1396=EDGE_LOOP('',(#5099,#5100,#5101,#5102));
#1397=EDGE_LOOP('',(#5103,#5104,#5105,#5106));
#1398=EDGE_LOOP('',(#5107,#5108,#5109,#5110,#5111,#5112,#5113,#5114,#5115,
#5116));
#1399=EDGE_LOOP('',(#5117,#5118,#5119,#5120));
#1400=EDGE_LOOP('',(#5121,#5122,#5123,#5124));
#1401=EDGE_LOOP('',(#5125,#5126,#5127,#5128));
#1402=EDGE_LOOP('',(#5129,#5130,#5131,#5132));
#1403=EDGE_LOOP('',(#5133,#5134,#5135,#5136));
#1404=EDGE_LOOP('',(#5137,#5138,#5139,#5140,#5141,#5142,#5143,#5144,#5145,
#5146));
#1405=EDGE_LOOP('',(#5147,#5148,#5149,#5150));
#1406=EDGE_LOOP('',(#5151,#5152,#5153,#5154,#5155,#5156));
#1407=EDGE_LOOP('',(#5157,#5158,#5159,#5160,#5161,#5162,#5163,#5164));
#1408=EDGE_LOOP('',(#5165));
#1409=EDGE_LOOP('',(#5166));
#1410=EDGE_LOOP('',(#5167));
#1411=EDGE_LOOP('',(#5168,#5169,#5170,#5171));
#1412=EDGE_LOOP('',(#5172,#5173,#5174,#5175,#5176,#5177,#5178,#5179,#5180,
#5181));
#1413=EDGE_LOOP('',(#5182,#5183,#5184,#5185));
#1414=EDGE_LOOP('',(#5186,#5187,#5188,#5189));
#1415=EDGE_LOOP('',(#5190,#5191,#5192,#5193));
#1416=EDGE_LOOP('',(#5194,#5195,#5196,#5197));
#1417=EDGE_LOOP('',(#5198,#5199,#5200,#5201));
#1418=EDGE_LOOP('',(#5202,#5203,#5204));
#1419=EDGE_LOOP('',(#5205,#5206,#5207));
#1420=EDGE_LOOP('',(#5208,#5209,#5210));
#1421=EDGE_LOOP('',(#5211,#5212,#5213,#5214));
#1422=EDGE_LOOP('',(#5215,#5216,#5217,#5218));
#1423=EDGE_LOOP('',(#5219,#5220,#5221));
#1424=EDGE_LOOP('',(#5222,#5223,#5224,#5225));
#1425=EDGE_LOOP('',(#5226,#5227,#5228,#5229));
#1426=EDGE_LOOP('',(#5230,#5231,#5232,#5233));
#1427=EDGE_LOOP('',(#5234,#5235,#5236,#5237));
#1428=EDGE_LOOP('',(#5238,#5239,#5240,#5241));
#1429=EDGE_LOOP('',(#5242,#5243,#5244,#5245));
#1430=EDGE_LOOP('',(#5246,#5247,#5248));
#1431=EDGE_LOOP('',(#5249,#5250,#5251));
#1432=EDGE_LOOP('',(#5252,#5253,#5254));
#1433=EDGE_LOOP('',(#5255,#5256,#5257,#5258));
#1434=EDGE_LOOP('',(#5259,#5260,#5261,#5262));
#1435=EDGE_LOOP('',(#5263,#5264,#5265));
#1436=EDGE_LOOP('',(#5266,#5267,#5268,#5269));
#1437=EDGE_LOOP('',(#5270,#5271,#5272,#5273));
#1438=EDGE_LOOP('',(#5274,#5275,#5276,#5277));
#1439=EDGE_LOOP('',(#5278,#5279,#5280,#5281));
#1440=EDGE_LOOP('',(#5282,#5283,#5284,#5285));
#1441=EDGE_LOOP('',(#5286,#5287,#5288,#5289));
#1442=EDGE_LOOP('',(#5290,#5291,#5292,#5293));
#1443=EDGE_LOOP('',(#5294,#5295,#5296,#5297,#5298,#5299,#5300,#5301));
#1444=EDGE_LOOP('',(#5302,#5303,#5304,#5305));
#1445=EDGE_LOOP('',(#5306,#5307,#5308,#5309,#5310,#5311));
#1446=EDGE_LOOP('',(#5312,#5313,#5314,#5315,#5316,#5317));
#1447=EDGE_LOOP('',(#5318));
#1448=EDGE_LOOP('',(#5319));
#1449=EDGE_LOOP('',(#5320));
#1450=EDGE_LOOP('',(#5321));
#1451=EDGE_LOOP('',(#5322,#5323,#5324,#5325));
#1452=EDGE_LOOP('',(#5326,#5327,#5328,#5329));
#1453=EDGE_LOOP('',(#5330,#5331,#5332,#5333));
#1454=EDGE_LOOP('',(#5334,#5335,#5336,#5337));
#1455=EDGE_LOOP('',(#5338,#5339,#5340,#5341));
#1456=EDGE_LOOP('',(#5342,#5343,#5344,#5345));
#1457=EDGE_LOOP('',(#5346,#5347,#5348,#5349));
#1458=EDGE_LOOP('',(#5350,#5351,#5352,#5353));
#1459=EDGE_LOOP('',(#5354,#5355,#5356,#5357));
#1460=EDGE_LOOP('',(#5358,#5359,#5360,#5361));
#1461=EDGE_LOOP('',(#5362,#5363,#5364,#5365));
#1462=EDGE_LOOP('',(#5366,#5367,#5368,#5369));
#1463=EDGE_LOOP('',(#5370,#5371,#5372,#5373));
#1464=EDGE_LOOP('',(#5374,#5375,#5376,#5377));
#1465=EDGE_LOOP('',(#5378,#5379,#5380,#5381));
#1466=EDGE_LOOP('',(#5382,#5383,#5384,#5385));
#1467=EDGE_LOOP('',(#5386,#5387,#5388,#5389));
#1468=EDGE_LOOP('',(#5390,#5391,#5392,#5393));
#1469=EDGE_LOOP('',(#5394,#5395,#5396,#5397));
#1470=EDGE_LOOP('',(#5398,#5399,#5400,#5401));
#1471=EDGE_LOOP('',(#5402,#5403,#5404,#5405));
#1472=EDGE_LOOP('',(#5406,#5407,#5408,#5409));
#1473=EDGE_LOOP('',(#5410,#5411,#5412,#5413));
#1474=EDGE_LOOP('',(#5414,#5415,#5416,#5417));
#1475=EDGE_LOOP('',(#5418,#5419,#5420,#5421));
#1476=EDGE_LOOP('',(#5422,#5423,#5424,#5425));
#1477=EDGE_LOOP('',(#5426,#5427,#5428,#5429));
#1478=EDGE_LOOP('',(#5430,#5431,#5432,#5433));
#1479=EDGE_LOOP('',(#5434,#5435,#5436,#5437));
#1480=EDGE_LOOP('',(#5438,#5439,#5440,#5441));
#1481=EDGE_LOOP('',(#5442,#5443,#5444,#5445));
#1482=EDGE_LOOP('',(#5446,#5447,#5448,#5449));
#1483=EDGE_LOOP('',(#5450,#5451,#5452,#5453));
#1484=EDGE_LOOP('',(#5454,#5455,#5456,#5457));
#1485=EDGE_LOOP('',(#5458,#5459,#5460,#5461));
#1486=EDGE_LOOP('',(#5462,#5463,#5464,#5465));
#1487=EDGE_LOOP('',(#5466,#5467,#5468,#5469));
#1488=EDGE_LOOP('',(#5470,#5471,#5472,#5473));
#1489=EDGE_LOOP('',(#5474,#5475,#5476,#5477));
#1490=EDGE_LOOP('',(#5478,#5479,#5480,#5481));
#1491=EDGE_LOOP('',(#5482,#5483,#5484,#5485));
#1492=EDGE_LOOP('',(#5486,#5487,#5488,#5489));
#1493=EDGE_LOOP('',(#5490,#5491,#5492,#5493));
#1494=EDGE_LOOP('',(#5494,#5495,#5496,#5497));
#1495=EDGE_LOOP('',(#5498,#5499,#5500,#5501));
#1496=EDGE_LOOP('',(#5502,#5503,#5504,#5505));
#1497=EDGE_LOOP('',(#5506,#5507,#5508,#5509));
#1498=EDGE_LOOP('',(#5510,#5511,#5512,#5513));
#1499=EDGE_LOOP('',(#5514,#5515,#5516,#5517));
#1500=EDGE_LOOP('',(#5518,#5519,#5520,#5521));
#1501=EDGE_LOOP('',(#5522,#5523,#5524,#5525));
#1502=EDGE_LOOP('',(#5526,#5527,#5528,#5529));
#1503=EDGE_LOOP('',(#5530,#5531,#5532,#5533));
#1504=EDGE_LOOP('',(#5534,#5535,#5536,#5537));
#1505=EDGE_LOOP('',(#5538,#5539,#5540,#5541));
#1506=EDGE_LOOP('',(#5542,#5543,#5544,#5545));
#1507=EDGE_LOOP('',(#5546,#5547,#5548,#5549));
#1508=EDGE_LOOP('',(#5550,#5551,#5552,#5553));
#1509=EDGE_LOOP('',(#5554,#5555,#5556,#5557));
#1510=EDGE_LOOP('',(#5558,#5559,#5560,#5561));
#1511=EDGE_LOOP('',(#5562,#5563,#5564,#5565));
#1512=EDGE_LOOP('',(#5566,#5567,#5568,#5569));
#1513=EDGE_LOOP('',(#5570,#5571,#5572,#5573,#5574,#5575,#5576,#5577));
#1514=EDGE_LOOP('',(#5578,#5579,#5580,#5581,#5582,#5583,#5584,#5585,#5586,
#5587,#5588,#5589,#5590,#5591,#5592,#5593,#5594,#5595,#5596,#5597,#5598,
#5599,#5600,#5601,#5602,#5603,#5604,#5605,#5606,#5607,#5608,#5609,#5610,
#5611,#5612,#5613,#5614,#5615,#5616,#5617,#5618,#5619,#5620,#5621,#5622,
#5623,#5624,#5625,#5626,#5627,#5628,#5629,#5630,#5631,#5632,#5633,#5634,
#5635,#5636,#5637,#5638,#5639,#5640,#5641));
#1515=EDGE_LOOP('',(#5642,#5643,#5644,#5645));
#1516=EDGE_LOOP('',(#5646,#5647,#5648,#5649,#5650,#5651,#5652,#5653,#5654,
#5655,#5656,#5657,#5658,#5659,#5660,#5661,#5662,#5663,#5664,#5665,#5666,
#5667,#5668,#5669,#5670,#5671,#5672,#5673,#5674,#5675,#5676,#5677,#5678,
#5679,#5680,#5681,#5682,#5683,#5684,#5685,#5686,#5687,#5688,#5689,#5690,
#5691,#5692,#5693,#5694,#5695,#5696,#5697,#5698,#5699,#5700,#5701,#5702,
#5703,#5704,#5705,#5706,#5707,#5708,#5709,#5710));
#1517=EDGE_LOOP('',(#5711,#5712,#5713,#5714));
#1518=EDGE_LOOP('',(#5715,#5716,#5717,#5718));
#1519=EDGE_LOOP('',(#5719,#5720,#5721,#5722));
#1520=EDGE_LOOP('',(#5723,#5724,#5725,#5726));
#1521=EDGE_LOOP('',(#5727,#5728,#5729,#5730));
#1522=EDGE_LOOP('',(#5731,#5732,#5733,#5734));
#1523=EDGE_LOOP('',(#5735,#5736,#5737,#5738));
#1524=EDGE_LOOP('',(#5739,#5740,#5741,#5742,#5743,#5744));
#1525=EDGE_LOOP('',(#5745));
#1526=EDGE_LOOP('',(#5746,#5747,#5748,#5749));
#1527=EDGE_LOOP('',(#5750,#5751,#5752,#5753));
#1528=EDGE_LOOP('',(#5754));
#1529=EDGE_LOOP('',(#5755,#5756,#5757,#5758,#5759,#5760));
#1530=EDGE_LOOP('',(#5761));
#1531=EDGE_LOOP('',(#5762,#5763,#5764));
#1532=EDGE_LOOP('',(#5765,#5766,#5767,#5768,#5769));
#1533=EDGE_LOOP('',(#5770,#5771,#5772,#5773));
#1534=EDGE_LOOP('',(#5774,#5775,#5776,#5777));
#1535=EDGE_LOOP('',(#5778,#5779,#5780,#5781));
#1536=EDGE_LOOP('',(#5782,#5783,#5784,#5785));
#1537=EDGE_LOOP('',(#5786,#5787,#5788,#5789));
#1538=EDGE_LOOP('',(#5790,#5791,#5792,#5793));
#1539=EDGE_LOOP('',(#5794,#5795,#5796,#5797));
#1540=EDGE_LOOP('',(#5798,#5799,#5800,#5801));
#1541=EDGE_LOOP('',(#5802,#5803,#5804,#5805));
#1542=EDGE_LOOP('',(#5806,#5807,#5808,#5809,#5810,#5811,#5812,#5813,#5814,
#5815,#5816,#5817,#5818,#5819));
#1543=EDGE_LOOP('',(#5820,#5821,#5822,#5823,#5824,#5825,#5826,#5827,#5828,
#5829,#5830,#5831,#5832));
#1544=EDGE_LOOP('',(#5833,#5834,#5835,#5836,#5837,#5838));
#1545=EDGE_LOOP('',(#5839,#5840,#5841,#5842));
#1546=EDGE_LOOP('',(#5843,#5844,#5845,#5846));
#1547=EDGE_LOOP('',(#5847,#5848,#5849,#5850));
#1548=EDGE_LOOP('',(#5851,#5852,#5853,#5854));
#1549=EDGE_LOOP('',(#5855,#5856,#5857,#5858));
#1550=EDGE_LOOP('',(#5859,#5860,#5861,#5862));
#1551=EDGE_LOOP('',(#5863,#5864,#5865,#5866));
#1552=EDGE_LOOP('',(#5867,#5868,#5869,#5870));
#1553=EDGE_LOOP('',(#5871,#5872,#5873,#5874,#5875,#5876));
#1554=EDGE_LOOP('',(#5877,#5878,#5879,#5880,#5881));
#1555=EDGE_LOOP('',(#5882,#5883,#5884,#5885));
#1556=EDGE_LOOP('',(#5886,#5887,#5888,#5889));
#1557=EDGE_LOOP('',(#5890));
#1558=EDGE_LOOP('',(#5891));
#1559=EDGE_LOOP('',(#5892,#5893,#5894,#5895));
#1560=EDGE_LOOP('',(#5896));
#1561=EDGE_LOOP('',(#5897));
#1562=EDGE_LOOP('',(#5898));
#1563=EDGE_LOOP('',(#5899,#5900,#5901,#5902));
#1564=EDGE_LOOP('',(#5903));
#1565=EDGE_LOOP('',(#5904));
#1566=EDGE_LOOP('',(#5905));
#1567=EDGE_LOOP('',(#5906,#5907,#5908,#5909));
#1568=EDGE_LOOP('',(#5910));
#1569=EDGE_LOOP('',(#5911));
#1570=EDGE_LOOP('',(#5912));
#1571=EDGE_LOOP('',(#5913,#5914,#5915,#5916));
#1572=EDGE_LOOP('',(#5917));
#1573=EDGE_LOOP('',(#5918,#5919,#5920,#5921));
#1574=EDGE_LOOP('',(#5922,#5923,#5924,#5925));
#1575=EDGE_LOOP('',(#5926,#5927,#5928,#5929));
#1576=EDGE_LOOP('',(#5930,#5931,#5932,#5933));
#1577=EDGE_LOOP('',(#5934,#5935,#5936,#5937));
#1578=EDGE_LOOP('',(#5938,#5939,#5940,#5941));
#1579=EDGE_LOOP('',(#5942,#5943,#5944,#5945));
#1580=EDGE_LOOP('',(#5946,#5947,#5948,#5949));
#1581=EDGE_LOOP('',(#5950,#5951,#5952,#5953));
#1582=EDGE_LOOP('',(#5954,#5955,#5956,#5957));
#1583=EDGE_LOOP('',(#5958,#5959,#5960,#5961));
#1584=EDGE_LOOP('',(#5962,#5963,#5964,#5965));
#1585=EDGE_LOOP('',(#5966,#5967,#5968,#5969));
#1586=EDGE_LOOP('',(#5970,#5971,#5972,#5973));
#1587=EDGE_LOOP('',(#5974,#5975,#5976,#5977));
#1588=EDGE_LOOP('',(#5978,#5979,#5980,#5981));
#1589=EDGE_LOOP('',(#5982,#5983,#5984,#5985,#5986,#5987,#5988,#5989));
#1590=EDGE_LOOP('',(#5990));
#1591=EDGE_LOOP('',(#5991));
#1592=EDGE_LOOP('',(#5992,#5993,#5994,#5995));
#1593=EDGE_LOOP('',(#5996,#5997,#5998,#5999));
#1594=EDGE_LOOP('',(#6000,#6001,#6002,#6003));
#1595=EDGE_LOOP('',(#6004,#6005,#6006,#6007,#6008,#6009,#6010,#6011));
#1596=EDGE_LOOP('',(#6012));
#1597=EDGE_LOOP('',(#6013));
#1598=EDGE_LOOP('',(#6014));
#1599=EDGE_LOOP('',(#6015));
#1600=EDGE_LOOP('',(#6016));
#1601=EDGE_LOOP('',(#6017));
#1602=EDGE_LOOP('',(#6018,#6019,#6020,#6021));
#1603=EDGE_LOOP('',(#6022,#6023,#6024,#6025));
#1604=EDGE_LOOP('',(#6026,#6027,#6028,#6029));
#1605=EDGE_LOOP('',(#6030));
#1606=EDGE_LOOP('',(#6031));
#1607=EDGE_LOOP('',(#6032));
#1608=EDGE_LOOP('',(#6033));
#1609=LINE('',#8509,#2016);
#1610=LINE('',#8515,#2017);
#1611=LINE('',#8521,#2018);
#1612=LINE('',#8526,#2019);
#1613=LINE('',#8528,#2020);
#1614=LINE('',#8529,#2021);
#1615=LINE('',#8533,#2022);
#1616=LINE('',#8535,#2023);
#1617=LINE('',#8536,#2024);
#1618=LINE('',#8537,#2025);
#1619=LINE('',#8540,#2026);
#1620=LINE('',#8542,#2027);
#1621=LINE('',#8543,#2028);
#1622=LINE('',#8546,#2029);
#1623=LINE('',#8547,#2030);
#1624=LINE('',#8550,#2031);
#1625=LINE('',#8552,#2032);
#1626=LINE('',#8554,#2033);
#1627=LINE('',#8556,#2034);
#1628=LINE('',#8557,#2035);
#1629=LINE('',#8560,#2036);
#1630=LINE('',#8562,#2037);
#1631=LINE('',#8563,#2038);
#1632=LINE('',#8566,#2039);
#1633=LINE('',#8567,#2040);
#1634=LINE('',#8570,#2041);
#1635=LINE('',#8571,#2042);
#1636=LINE('',#8574,#2043);
#1637=LINE('',#8575,#2044);
#1638=LINE('',#8577,#2045);
#1639=LINE('',#8580,#2046);
#1640=LINE('',#8582,#2047);
#1641=LINE('',#8584,#2048);
#1642=LINE('',#8588,#2049);
#1643=LINE('',#8590,#2050);
#1644=LINE('',#8592,#2051);
#1645=LINE('',#8594,#2052);
#1646=LINE('',#8596,#2053);
#1647=LINE('',#8598,#2054);
#1648=LINE('',#8602,#2055);
#1649=LINE('',#8603,#2056);
#1650=LINE('',#8606,#2057);
#1651=LINE('',#8608,#2058);
#1652=LINE('',#8609,#2059);
#1653=LINE('',#8612,#2060);
#1654=LINE('',#8613,#2061);
#1655=LINE('',#8616,#2062);
#1656=LINE('',#8617,#2063);
#1657=LINE('',#8620,#2064);
#1658=LINE('',#8621,#2065);
#1659=LINE('',#8624,#2066);
#1660=LINE('',#8629,#2067);
#1661=LINE('',#8632,#2068);
#1662=LINE('',#8634,#2069);
#1663=LINE('',#8636,#2070);
#1664=LINE('',#8638,#2071);
#1665=LINE('',#8640,#2072);
#1666=LINE('',#8641,#2073);
#1667=LINE('',#8643,#2074);
#1668=LINE('',#8645,#2075);
#1669=LINE('',#8647,#2076);
#1670=LINE('',#8649,#2077);
#1671=LINE('',#8651,#2078);
#1672=LINE('',#8658,#2079);
#1673=LINE('',#8669,#2080);
#1674=LINE('',#8677,#2081);
#1675=LINE('',#8681,#2082);
#1676=LINE('',#8687,#2083);
#1677=LINE('',#8689,#2084);
#1678=LINE('',#8691,#2085);
#1679=LINE('',#8692,#2086);
#1680=LINE('',#8696,#2087);
#1681=LINE('',#8698,#2088);
#1682=LINE('',#8700,#2089);
#1683=LINE('',#8701,#2090);
#1684=LINE('',#9006,#2091);
#1685=LINE('',#9008,#2092);
#1686=LINE('',#9022,#2093);
#1687=LINE('',#9027,#2094);
#1688=LINE('',#9033,#2095);
#1689=LINE('',#9038,#2096);
#1690=LINE('',#9043,#2097);
#1691=LINE('',#9052,#2098);
#1692=LINE('',#9059,#2099);
#1693=LINE('',#9063,#2100);
#1694=LINE('',#9068,#2101);
#1695=LINE('',#9070,#2102);
#1696=LINE('',#9072,#2103);
#1697=LINE('',#9073,#2104);
#1698=LINE('',#9077,#2105);
#1699=LINE('',#9079,#2106);
#1700=LINE('',#9081,#2107);
#1701=LINE('',#9082,#2108);
#1702=LINE('',#9086,#2109);
#1703=LINE('',#9088,#2110);
#1704=LINE('',#9090,#2111);
#1705=LINE('',#9091,#2112);
#1706=LINE('',#9095,#2113);
#1707=LINE('',#9097,#2114);
#1708=LINE('',#9099,#2115);
#1709=LINE('',#9100,#2116);
#1710=LINE('',#9104,#2117);
#1711=LINE('',#9106,#2118);
#1712=LINE('',#9108,#2119);
#1713=LINE('',#9109,#2120);
#1714=LINE('',#9113,#2121);
#1715=LINE('',#9115,#2122);
#1716=LINE('',#9117,#2123);
#1717=LINE('',#9118,#2124);
#1718=LINE('',#9122,#2125);
#1719=LINE('',#9124,#2126);
#1720=LINE('',#9126,#2127);
#1721=LINE('',#9127,#2128);
#1722=LINE('',#9135,#2129);
#1723=LINE('',#9136,#2130);
#1724=LINE('',#9138,#2131);
#1725=LINE('',#9139,#2132);
#1726=LINE('',#9141,#2133);
#1727=LINE('',#9142,#2134);
#1728=LINE('',#9145,#2135);
#1729=LINE('',#9147,#2136);
#1730=LINE('',#9148,#2137);
#1731=LINE('',#9151,#2138);
#1732=LINE('',#9153,#2139);
#1733=LINE('',#9154,#2140);
#1734=LINE('',#9158,#2141);
#1735=LINE('',#9202,#2142);
#1736=LINE('',#9245,#2143);
#1737=LINE('',#9248,#2144);
#1738=LINE('',#9286,#2145);
#1739=LINE('',#9323,#2146);
#1740=LINE('',#9326,#2147);
#1741=LINE('',#9334,#2148);
#1742=LINE('',#9371,#2149);
#1743=LINE('',#9374,#2150);
#1744=LINE('',#9381,#2151);
#1745=LINE('',#9387,#2152);
#1746=LINE('',#9398,#2153);
#1747=LINE('',#9407,#2154);
#1748=LINE('',#9413,#2155);
#1749=LINE('',#9448,#2156);
#1750=LINE('',#9519,#2157);
#1751=LINE('',#9589,#2158);
#1752=LINE('',#9621,#2159);
#1753=LINE('',#9627,#2160);
#1754=LINE('',#9636,#2161);
#1755=LINE('',#9673,#2162);
#1756=LINE('',#9708,#2163);
#1757=LINE('',#9710,#2164);
#1758=LINE('',#9714,#2165);
#1759=LINE('',#9760,#2166);
#1760=LINE('',#9886,#2167);
#1761=LINE('',#9966,#2168);
#1762=LINE('',#10128,#2169);
#1763=LINE('',#10238,#2170);
#1764=LINE('',#10327,#2171);
#1765=LINE('',#10415,#2172);
#1766=LINE('',#10527,#2173);
#1767=LINE('',#10528,#2174);
#1768=LINE('',#10565,#2175);
#1769=LINE('',#10566,#2176);
#1770=LINE('',#11051,#2177);
#1771=LINE('',#11053,#2178);
#1772=LINE('',#11067,#2179);
#1773=LINE('',#11069,#2180);
#1774=LINE('',#11071,#2181);
#1775=LINE('',#11072,#2182);
#1776=LINE('',#11075,#2183);
#1777=LINE('',#11077,#2184);
#1778=LINE('',#11078,#2185);
#1779=LINE('',#11081,#2186);
#1780=LINE('',#11083,#2187);
#1781=LINE('',#11084,#2188);
#1782=LINE('',#11087,#2189);
#1783=LINE('',#11089,#2190);
#1784=LINE('',#11090,#2191);
#1785=LINE('',#11093,#2192);
#1786=LINE('',#11095,#2193);
#1787=LINE('',#11096,#2194);
#1788=LINE('',#11098,#2195);
#1789=LINE('',#11099,#2196);
#1790=LINE('',#11106,#2197);
#1791=LINE('',#11108,#2198);
#1792=LINE('',#11110,#2199);
#1793=LINE('',#11111,#2200);
#1794=LINE('',#11114,#2201);
#1795=LINE('',#11116,#2202);
#1796=LINE('',#11117,#2203);
#1797=LINE('',#11120,#2204);
#1798=LINE('',#11122,#2205);
#1799=LINE('',#11123,#2206);
#1800=LINE('',#11126,#2207);
#1801=LINE('',#11128,#2208);
#1802=LINE('',#11129,#2209);
#1803=LINE('',#11132,#2210);
#1804=LINE('',#11134,#2211);
#1805=LINE('',#11135,#2212);
#1806=LINE('',#11137,#2213);
#1807=LINE('',#11138,#2214);
#1808=LINE('',#11145,#2215);
#1809=LINE('',#11150,#2216);
#1810=LINE('',#11156,#2217);
#1811=LINE('',#11161,#2218);
#1812=LINE('',#11164,#2219);
#1813=LINE('',#11168,#2220);
#1814=LINE('',#11173,#2221);
#1815=LINE('',#11175,#2222);
#1816=LINE('',#11177,#2223);
#1817=LINE('',#11178,#2224);
#1818=LINE('',#11182,#2225);
#1819=LINE('',#11184,#2226);
#1820=LINE('',#11186,#2227);
#1821=LINE('',#11187,#2228);
#1822=LINE('',#11191,#2229);
#1823=LINE('',#11193,#2230);
#1824=LINE('',#11195,#2231);
#1825=LINE('',#11196,#2232);
#1826=LINE('',#11200,#2233);
#1827=LINE('',#11202,#2234);
#1828=LINE('',#11204,#2235);
#1829=LINE('',#11205,#2236);
#1830=LINE('',#11209,#2237);
#1831=LINE('',#11211,#2238);
#1832=LINE('',#11213,#2239);
#1833=LINE('',#11214,#2240);
#1834=LINE('',#11218,#2241);
#1835=LINE('',#11220,#2242);
#1836=LINE('',#11222,#2243);
#1837=LINE('',#11223,#2244);
#1838=LINE('',#11227,#2245);
#1839=LINE('',#11229,#2246);
#1840=LINE('',#11231,#2247);
#1841=LINE('',#11232,#2248);
#1842=LINE('',#11240,#2249);
#1843=LINE('',#11241,#2250);
#1844=LINE('',#11243,#2251);
#1845=LINE('',#11244,#2252);
#1846=LINE('',#11246,#2253);
#1847=LINE('',#11247,#2254);
#1848=LINE('',#11250,#2255);
#1849=LINE('',#11252,#2256);
#1850=LINE('',#11253,#2257);
#1851=LINE('',#11256,#2258);
#1852=LINE('',#11258,#2259);
#1853=LINE('',#11259,#2260);
#1854=LINE('',#11263,#2261);
#1855=LINE('',#11307,#2262);
#1856=LINE('',#11350,#2263);
#1857=LINE('',#11353,#2264);
#1858=LINE('',#11391,#2265);
#1859=LINE('',#11428,#2266);
#1860=LINE('',#11431,#2267);
#1861=LINE('',#11439,#2268);
#1862=LINE('',#11476,#2269);
#1863=LINE('',#11479,#2270);
#1864=LINE('',#11486,#2271);
#1865=LINE('',#11492,#2272);
#1866=LINE('',#11503,#2273);
#1867=LINE('',#11512,#2274);
#1868=LINE('',#11518,#2275);
#1869=LINE('',#11553,#2276);
#1870=LINE('',#11624,#2277);
#1871=LINE('',#11694,#2278);
#1872=LINE('',#11726,#2279);
#1873=LINE('',#11732,#2280);
#1874=LINE('',#11741,#2281);
#1875=LINE('',#11778,#2282);
#1876=LINE('',#11813,#2283);
#1877=LINE('',#11815,#2284);
#1878=LINE('',#11819,#2285);
#1879=LINE('',#11865,#2286);
#1880=LINE('',#11991,#2287);
#1881=LINE('',#12071,#2288);
#1882=LINE('',#12233,#2289);
#1883=LINE('',#12343,#2290);
#1884=LINE('',#12432,#2291);
#1885=LINE('',#12520,#2292);
#1886=LINE('',#12632,#2293);
#1887=LINE('',#12633,#2294);
#1888=LINE('',#12670,#2295);
#1889=LINE('',#12671,#2296);
#1890=LINE('',#12865,#2297);
#1891=LINE('',#12889,#2298);
#1892=LINE('',#12937,#2299);
#1893=LINE('',#12985,#2300);
#1894=LINE('',#13036,#2301);
#1895=LINE('',#13084,#2302);
#1896=LINE('',#13132,#2303);
#1897=LINE('',#13180,#2304);
#1898=LINE('',#13234,#2305);
#1899=LINE('',#13282,#2306);
#1900=LINE('',#13330,#2307);
#1901=LINE('',#13384,#2308);
#1902=LINE('',#13432,#2309);
#1903=LINE('',#13480,#2310);
#1904=LINE('',#13528,#2311);
#1905=LINE('',#13582,#2312);
#1906=LINE('',#13630,#2313);
#1907=LINE('',#13678,#2314);
#1908=LINE('',#13732,#2315);
#1909=LINE('',#13780,#2316);
#1910=LINE('',#13828,#2317);
#1911=LINE('',#13882,#2318);
#1912=LINE('',#13930,#2319);
#1913=LINE('',#13978,#2320);
#1914=LINE('',#14026,#2321);
#1915=LINE('',#14080,#2322);
#1916=LINE('',#14128,#2323);
#1917=LINE('',#14176,#2324);
#1918=LINE('',#14230,#2325);
#1919=LINE('',#14278,#2326);
#1920=LINE('',#14326,#2327);
#1921=LINE('',#14352,#2328);
#1922=LINE('',#14376,#2329);
#1923=LINE('',#14400,#2330);
#1924=LINE('',#14425,#2331);
#1925=LINE('',#14450,#2332);
#1926=LINE('',#14474,#2333);
#1927=LINE('',#14499,#2334);
#1928=LINE('',#14524,#2335);
#1929=LINE('',#14548,#2336);
#1930=LINE('',#14572,#2337);
#1931=LINE('',#14597,#2338);
#1932=LINE('',#14622,#2339);
#1933=LINE('',#14646,#2340);
#1934=LINE('',#14671,#2341);
#1935=LINE('',#14696,#2342);
#1936=LINE('',#14720,#2343);
#1937=LINE('',#14745,#2344);
#1938=LINE('',#14770,#2345);
#1939=LINE('',#14794,#2346);
#1940=LINE('',#14818,#2347);
#1941=LINE('',#14843,#2348);
#1942=LINE('',#14868,#2349);
#1943=LINE('',#14892,#2350);
#1944=LINE('',#14917,#2351);
#1945=LINE('',#14942,#2352);
#1946=LINE('',#14966,#2353);
#1947=LINE('',#14991,#2354);
#1948=LINE('',#15015,#2355);
#1949=LINE('',#15040,#2356);
#1950=LINE('',#15241,#2357);
#1951=LINE('',#16986,#2358);
#1952=LINE('',#16988,#2359);
#1953=LINE('',#16990,#2360);
#1954=LINE('',#16991,#2361);
#1955=LINE('',#16994,#2362);
#1956=LINE('',#16996,#2363);
#1957=LINE('',#16997,#2364);
#1958=LINE('',#17000,#2365);
#1959=LINE('',#17002,#2366);
#1960=LINE('',#17003,#2367);
#1961=LINE('',#17006,#2368);
#1962=LINE('',#17008,#2369);
#1963=LINE('',#17009,#2370);
#1964=LINE('',#17012,#2371);
#1965=LINE('',#17014,#2372);
#1966=LINE('',#17015,#2373);
#1967=LINE('',#17017,#2374);
#1968=LINE('',#17018,#2375);
#1969=LINE('',#17025,#2376);
#1970=LINE('',#17033,#2377);
#1971=LINE('',#17046,#2378);
#1972=LINE('',#17093,#2379);
#1973=LINE('',#17147,#2380);
#1974=LINE('',#17195,#2381);
#1975=LINE('',#17234,#2382);
#1976=LINE('',#17255,#2383);
#1977=LINE('',#17280,#2384);
#1978=LINE('',#17305,#2385);
#1979=LINE('',#17330,#2386);
#1980=LINE('',#17903,#2387);
#1981=LINE('',#17905,#2388);
#1982=LINE('',#17907,#2389);
#1983=LINE('',#17909,#2390);
#1984=LINE('',#17911,#2391);
#1985=LINE('',#17912,#2392);
#1986=LINE('',#17917,#2393);
#1987=LINE('',#17918,#2394);
#1988=LINE('',#17919,#2395);
#1989=LINE('',#17922,#2396);
#1990=LINE('',#17923,#2397);
#1991=LINE('',#17926,#2398);
#1992=LINE('',#17927,#2399);
#1993=LINE('',#17930,#2400);
#1994=LINE('',#17931,#2401);
#1995=LINE('',#17934,#2402);
#1996=LINE('',#17935,#2403);
#1997=LINE('',#17937,#2404);
#1998=LINE('',#17944,#2405);
#1999=LINE('',#17950,#2406);
#2000=LINE('',#17960,#2407);
#2001=LINE('',#17970,#2408);
#2002=LINE('',#17980,#2409);
#2003=LINE('',#17990,#2410);
#2004=LINE('',#17994,#2411);
#2005=LINE('',#17998,#2412);
#2006=LINE('',#18002,#2413);
#2007=LINE('',#18006,#2414);
#2008=LINE('',#18053,#2415);
#2009=LINE('',#18054,#2416);
#2010=LINE('',#18173,#2417);
#2011=LINE('',#18174,#2418);
#2012=LINE('',#18255,#2419);
#2013=LINE('',#18398,#2420);
#2014=LINE('',#18539,#2421);
#2015=LINE('',#18545,#2422);
#2016=VECTOR('',#7142,0.17);
#2017=VECTOR('',#7149,0.17);
#2018=VECTOR('',#7156,0.41);
#2019=VECTOR('',#7161,1.);
#2020=VECTOR('',#7162,1.);
#2021=VECTOR('',#7163,1.);
#2022=VECTOR('',#7166,1.);
#2023=VECTOR('',#7167,1.);
#2024=VECTOR('',#7168,1.);
#2025=VECTOR('',#7169,1.);
#2026=VECTOR('',#7172,1.);
#2027=VECTOR('',#7173,1.);
#2028=VECTOR('',#7174,1.);
#2029=VECTOR('',#7177,1.);
#2030=VECTOR('',#7178,1.);
#2031=VECTOR('',#7181,1.);
#2032=VECTOR('',#7182,1.);
#2033=VECTOR('',#7183,1.);
#2034=VECTOR('',#7184,1.);
#2035=VECTOR('',#7185,1.);
#2036=VECTOR('',#7188,1.);
#2037=VECTOR('',#7189,1.);
#2038=VECTOR('',#7190,1.);
#2039=VECTOR('',#7193,1.);
#2040=VECTOR('',#7194,1.);
#2041=VECTOR('',#7197,1.);
#2042=VECTOR('',#7198,1.);
#2043=VECTOR('',#7201,1.);
#2044=VECTOR('',#7202,1.);
#2045=VECTOR('',#7205,1.);
#2046=VECTOR('',#7208,1.);
#2047=VECTOR('',#7209,1.);
#2048=VECTOR('',#7210,1.);
#2049=VECTOR('',#7213,1.);
#2050=VECTOR('',#7214,1.);
#2051=VECTOR('',#7215,1.);
#2052=VECTOR('',#7216,1.);
#2053=VECTOR('',#7217,1.);
#2054=VECTOR('',#7218,1.);
#2055=VECTOR('',#7221,1.);
#2056=VECTOR('',#7222,1.);
#2057=VECTOR('',#7225,1.);
#2058=VECTOR('',#7226,1.);
#2059=VECTOR('',#7227,1.);
#2060=VECTOR('',#7230,1.);
#2061=VECTOR('',#7231,1.);
#2062=VECTOR('',#7234,1.);
#2063=VECTOR('',#7235,1.);
#2064=VECTOR('',#7238,1.);
#2065=VECTOR('',#7239,1.);
#2066=VECTOR('',#7242,1.);
#2067=VECTOR('',#7249,1.);
#2068=VECTOR('',#7252,1.);
#2069=VECTOR('',#7253,1.);
#2070=VECTOR('',#7254,1.);
#2071=VECTOR('',#7255,1.);
#2072=VECTOR('',#7256,1.);
#2073=VECTOR('',#7257,1.);
#2074=VECTOR('',#7260,1.);
#2075=VECTOR('',#7263,1.);
#2076=VECTOR('',#7266,1.);
#2077=VECTOR('',#7269,1.);
#2078=VECTOR('',#7272,1.);
#2079=VECTOR('',#7281,0.3);
#2080=VECTOR('',#7296,0.4);
#2081=VECTOR('',#7305,0.6);
#2082=VECTOR('',#7312,0.4);
#2083=VECTOR('',#7319,1.);
#2084=VECTOR('',#7320,1.);
#2085=VECTOR('',#7321,1.);
#2086=VECTOR('',#7322,1.);
#2087=VECTOR('',#7325,1.);
#2088=VECTOR('',#7326,1.);
#2089=VECTOR('',#7327,1.);
#2090=VECTOR('',#7328,1.);
#2091=VECTOR('',#7367,1.);
#2092=VECTOR('',#7368,1.);
#2093=VECTOR('',#7379,0.15);
#2094=VECTOR('',#7384,0.15);
#2095=VECTOR('',#7391,0.15);
#2096=VECTOR('',#7398,0.15);
#2097=VECTOR('',#7403,0.3);
#2098=VECTOR('',#7414,0.3);
#2099=VECTOR('',#7423,0.17);
#2100=VECTOR('',#7428,0.17);
#2101=VECTOR('',#7433,1.);
#2102=VECTOR('',#7434,1.);
#2103=VECTOR('',#7435,1.);
#2104=VECTOR('',#7436,1.);
#2105=VECTOR('',#7439,1.);
#2106=VECTOR('',#7440,1.);
#2107=VECTOR('',#7441,1.);
#2108=VECTOR('',#7442,1.);
#2109=VECTOR('',#7445,1.);
#2110=VECTOR('',#7446,1.);
#2111=VECTOR('',#7447,1.);
#2112=VECTOR('',#7448,1.);
#2113=VECTOR('',#7451,1.);
#2114=VECTOR('',#7452,1.);
#2115=VECTOR('',#7453,1.);
#2116=VECTOR('',#7454,1.);
#2117=VECTOR('',#7457,1.);
#2118=VECTOR('',#7458,1.);
#2119=VECTOR('',#7459,1.);
#2120=VECTOR('',#7460,1.);
#2121=VECTOR('',#7463,1.);
#2122=VECTOR('',#7464,1.);
#2123=VECTOR('',#7465,1.);
#2124=VECTOR('',#7466,1.);
#2125=VECTOR('',#7469,1.);
#2126=VECTOR('',#7470,1.);
#2127=VECTOR('',#7471,1.);
#2128=VECTOR('',#7472,1.);
#2129=VECTOR('',#7483,1.);
#2130=VECTOR('',#7484,1.);
#2131=VECTOR('',#7487,1.);
#2132=VECTOR('',#7488,1.);
#2133=VECTOR('',#7491,1.);
#2134=VECTOR('',#7492,1.);
#2135=VECTOR('',#7495,1.);
#2136=VECTOR('',#7496,1.);
#2137=VECTOR('',#7497,1.);
#2138=VECTOR('',#7500,1.);
#2139=VECTOR('',#7501,1.);
#2140=VECTOR('',#7502,1.);
#2141=VECTOR('',#7505,1.);
#2142=VECTOR('',#7508,1.);
#2143=VECTOR('',#7509,1.);
#2144=VECTOR('',#7512,1.);
#2145=VECTOR('',#7513,1.);
#2146=VECTOR('',#7514,1.);
#2147=VECTOR('',#7517,1.);
#2148=VECTOR('',#7518,1.);
#2149=VECTOR('',#7519,1.);
#2150=VECTOR('',#7522,1.);
#2151=VECTOR('',#7523,1.);
#2152=VECTOR('',#7524,1.);
#2153=VECTOR('',#7527,1.);
#2154=VECTOR('',#7528,1.);
#2155=VECTOR('',#7529,1.);
#2156=VECTOR('',#7530,1.);
#2157=VECTOR('',#7531,1.);
#2158=VECTOR('',#7532,1.);
#2159=VECTOR('',#7533,1.);
#2160=VECTOR('',#7534,1.);
#2161=VECTOR('',#7535,1.);
#2162=VECTOR('',#7536,1.);
#2163=VECTOR('',#7537,1.);
#2164=VECTOR('',#7540,0.4);
#2165=VECTOR('',#7545,0.4);
#2166=VECTOR('',#7548,1.);
#2167=VECTOR('',#7553,1.);
#2168=VECTOR('',#7556,1.);
#2169=VECTOR('',#7561,1.);
#2170=VECTOR('',#7566,1.);
#2171=VECTOR('',#7571,1.);
#2172=VECTOR('',#7604,1.);
#2173=VECTOR('',#7633,1.);
#2174=VECTOR('',#7634,1.);
#2175=VECTOR('',#7645,1.);
#2176=VECTOR('',#7646,1.);
#2177=VECTOR('',#7673,1.);
#2178=VECTOR('',#7674,1.);
#2179=VECTOR('',#7683,1.);
#2180=VECTOR('',#7684,1.);
#2181=VECTOR('',#7685,1.);
#2182=VECTOR('',#7686,1.);
#2183=VECTOR('',#7689,1.);
#2184=VECTOR('',#7690,1.);
#2185=VECTOR('',#7691,1.);
#2186=VECTOR('',#7694,1.);
#2187=VECTOR('',#7695,1.);
#2188=VECTOR('',#7696,1.);
#2189=VECTOR('',#7699,1.);
#2190=VECTOR('',#7700,1.);
#2191=VECTOR('',#7701,1.);
#2192=VECTOR('',#7704,1.);
#2193=VECTOR('',#7705,1.);
#2194=VECTOR('',#7706,1.);
#2195=VECTOR('',#7709,1.);
#2196=VECTOR('',#7710,1.);
#2197=VECTOR('',#7717,1.);
#2198=VECTOR('',#7718,1.);
#2199=VECTOR('',#7719,1.);
#2200=VECTOR('',#7720,1.);
#2201=VECTOR('',#7723,1.);
#2202=VECTOR('',#7724,1.);
#2203=VECTOR('',#7725,1.);
#2204=VECTOR('',#7728,1.);
#2205=VECTOR('',#7729,1.);
#2206=VECTOR('',#7730,1.);
#2207=VECTOR('',#7733,1.);
#2208=VECTOR('',#7734,1.);
#2209=VECTOR('',#7735,1.);
#2210=VECTOR('',#7738,1.);
#2211=VECTOR('',#7739,1.);
#2212=VECTOR('',#7740,1.);
#2213=VECTOR('',#7743,1.);
#2214=VECTOR('',#7744,1.);
#2215=VECTOR('',#7753,0.15);
#2216=VECTOR('',#7758,0.15);
#2217=VECTOR('',#7765,0.15);
#2218=VECTOR('',#7772,0.15);
#2219=VECTOR('',#7775,0.17);
#2220=VECTOR('',#7780,0.17);
#2221=VECTOR('',#7785,1.);
#2222=VECTOR('',#7786,1.);
#2223=VECTOR('',#7787,1.);
#2224=VECTOR('',#7788,1.);
#2225=VECTOR('',#7791,1.);
#2226=VECTOR('',#7792,1.);
#2227=VECTOR('',#7793,1.);
#2228=VECTOR('',#7794,1.);
#2229=VECTOR('',#7797,1.);
#2230=VECTOR('',#7798,1.);
#2231=VECTOR('',#7799,1.);
#2232=VECTOR('',#7800,1.);
#2233=VECTOR('',#7803,1.);
#2234=VECTOR('',#7804,1.);
#2235=VECTOR('',#7805,1.);
#2236=VECTOR('',#7806,1.);
#2237=VECTOR('',#7809,1.);
#2238=VECTOR('',#7810,1.);
#2239=VECTOR('',#7811,1.);
#2240=VECTOR('',#7812,1.);
#2241=VECTOR('',#7815,1.);
#2242=VECTOR('',#7816,1.);
#2243=VECTOR('',#7817,1.);
#2244=VECTOR('',#7818,1.);
#2245=VECTOR('',#7821,1.);
#2246=VECTOR('',#7822,1.);
#2247=VECTOR('',#7823,1.);
#2248=VECTOR('',#7824,1.);
#2249=VECTOR('',#7835,1.);
#2250=VECTOR('',#7836,1.);
#2251=VECTOR('',#7839,1.);
#2252=VECTOR('',#7840,1.);
#2253=VECTOR('',#7843,1.);
#2254=VECTOR('',#7844,1.);
#2255=VECTOR('',#7847,1.);
#2256=VECTOR('',#7848,1.);
#2257=VECTOR('',#7849,1.);
#2258=VECTOR('',#7852,1.);
#2259=VECTOR('',#7853,1.);
#2260=VECTOR('',#7854,1.);
#2261=VECTOR('',#7857,1.);
#2262=VECTOR('',#7860,1.);
#2263=VECTOR('',#7861,1.);
#2264=VECTOR('',#7864,1.);
#2265=VECTOR('',#7865,1.);
#2266=VECTOR('',#7866,1.);
#2267=VECTOR('',#7869,1.);
#2268=VECTOR('',#7870,1.);
#2269=VECTOR('',#7871,1.);
#2270=VECTOR('',#7874,1.);
#2271=VECTOR('',#7875,1.);
#2272=VECTOR('',#7876,1.);
#2273=VECTOR('',#7879,1.);
#2274=VECTOR('',#7880,1.);
#2275=VECTOR('',#7881,1.);
#2276=VECTOR('',#7882,1.);
#2277=VECTOR('',#7883,1.);
#2278=VECTOR('',#7884,1.);
#2279=VECTOR('',#7885,1.);
#2280=VECTOR('',#7886,1.);
#2281=VECTOR('',#7887,1.);
#2282=VECTOR('',#7888,1.);
#2283=VECTOR('',#7889,1.);
#2284=VECTOR('',#7892,0.4);
#2285=VECTOR('',#7897,0.4);
#2286=VECTOR('',#7900,1.);
#2287=VECTOR('',#7905,1.);
#2288=VECTOR('',#7908,1.);
#2289=VECTOR('',#7913,1.);
#2290=VECTOR('',#7918,1.);
#2291=VECTOR('',#7923,1.);
#2292=VECTOR('',#7956,1.);
#2293=VECTOR('',#7985,1.);
#2294=VECTOR('',#7986,1.);
#2295=VECTOR('',#7997,1.);
#2296=VECTOR('',#7998,1.);
#2297=VECTOR('',#8009,0.15);
#2298=VECTOR('',#8014,0.15);
#2299=VECTOR('',#8017,0.15);
#2300=VECTOR('',#8020,0.15);
#2301=VECTOR('',#8023,0.15);
#2302=VECTOR('',#8026,0.15);
#2303=VECTOR('',#8029,0.15);
#2304=VECTOR('',#8032,0.15);
#2305=VECTOR('',#8035,0.15);
#2306=VECTOR('',#8038,0.15);
#2307=VECTOR('',#8041,0.15);
#2308=VECTOR('',#8044,0.15);
#2309=VECTOR('',#8047,0.15);
#2310=VECTOR('',#8050,0.15);
#2311=VECTOR('',#8053,0.15);
#2312=VECTOR('',#8056,0.15);
#2313=VECTOR('',#8059,0.15);
#2314=VECTOR('',#8062,0.15);
#2315=VECTOR('',#8065,0.15);
#2316=VECTOR('',#8068,0.15);
#2317=VECTOR('',#8071,0.15);
#2318=VECTOR('',#8074,0.15);
#2319=VECTOR('',#8077,0.15);
#2320=VECTOR('',#8080,0.15);
#2321=VECTOR('',#8083,0.15);
#2322=VECTOR('',#8086,0.15);
#2323=VECTOR('',#8089,0.15);
#2324=VECTOR('',#8092,0.15);
#2325=VECTOR('',#8095,0.15);
#2326=VECTOR('',#8098,0.15);
#2327=VECTOR('',#8101,0.117775);
#2328=VECTOR('',#8106,0.117775);
#2329=VECTOR('',#8109,0.117775);
#2330=VECTOR('',#8112,0.117775);
#2331=VECTOR('',#8115,0.117775);
#2332=VECTOR('',#8118,0.117775);
#2333=VECTOR('',#8121,0.117775);
#2334=VECTOR('',#8124,0.117775);
#2335=VECTOR('',#8127,0.117775);
#2336=VECTOR('',#8130,0.117775);
#2337=VECTOR('',#8133,0.117775);
#2338=VECTOR('',#8136,0.117775);
#2339=VECTOR('',#8139,0.117775);
#2340=VECTOR('',#8142,0.117775);
#2341=VECTOR('',#8145,0.117775);
#2342=VECTOR('',#8148,0.117775);
#2343=VECTOR('',#8151,0.117775);
#2344=VECTOR('',#8154,0.117775);
#2345=VECTOR('',#8157,0.117775);
#2346=VECTOR('',#8160,0.117775);
#2347=VECTOR('',#8163,0.117775);
#2348=VECTOR('',#8166,0.117775);
#2349=VECTOR('',#8169,0.117775);
#2350=VECTOR('',#8172,0.117775);
#2351=VECTOR('',#8175,0.117775);
#2352=VECTOR('',#8178,0.117775);
#2353=VECTOR('',#8181,0.117775);
#2354=VECTOR('',#8184,0.117775);
#2355=VECTOR('',#8187,0.117775);
#2356=VECTOR('',#8190,0.117775);
#2357=VECTOR('',#8195,0.1);
#2358=VECTOR('',#8206,1.);
#2359=VECTOR('',#8207,1.);
#2360=VECTOR('',#8208,1.);
#2361=VECTOR('',#8209,1.);
#2362=VECTOR('',#8212,1.);
#2363=VECTOR('',#8213,1.);
#2364=VECTOR('',#8214,1.);
#2365=VECTOR('',#8217,1.);
#2366=VECTOR('',#8218,1.);
#2367=VECTOR('',#8219,1.);
#2368=VECTOR('',#8222,1.);
#2369=VECTOR('',#8223,1.);
#2370=VECTOR('',#8224,1.);
#2371=VECTOR('',#8227,1.);
#2372=VECTOR('',#8228,1.);
#2373=VECTOR('',#8229,1.);
#2374=VECTOR('',#8232,1.);
#2375=VECTOR('',#8233,1.);
#2376=VECTOR('',#8242,0.275);
#2377=VECTOR('',#8253,0.15);
#2378=VECTOR('',#8258,0.15);
#2379=VECTOR('',#8263,0.15);
#2380=VECTOR('',#8266,0.15);
#2381=VECTOR('',#8269,0.15);
#2382=VECTOR('',#8274,0.1543);
#2383=VECTOR('',#8279,0.1543);
#2384=VECTOR('',#8282,0.1543);
#2385=VECTOR('',#8285,0.1543);
#2386=VECTOR('',#8288,0.1543);
#2387=VECTOR('',#8295,1.);
#2388=VECTOR('',#8296,1.);
#2389=VECTOR('',#8297,1.);
#2390=VECTOR('',#8298,1.);
#2391=VECTOR('',#8299,1.);
#2392=VECTOR('',#8300,1.);
#2393=VECTOR('',#8305,1.);
#2394=VECTOR('',#8306,1.);
#2395=VECTOR('',#8307,1.);
#2396=VECTOR('',#8310,1.);
#2397=VECTOR('',#8311,1.);
#2398=VECTOR('',#8314,1.);
#2399=VECTOR('',#8315,1.);
#2400=VECTOR('',#8318,1.);
#2401=VECTOR('',#8319,1.);
#2402=VECTOR('',#8322,1.);
#2403=VECTOR('',#8323,1.);
#2404=VECTOR('',#8326,1.);
#2405=VECTOR('',#8335,0.35);
#2406=VECTOR('',#8342,0.35);
#2407=VECTOR('',#8355,0.25);
#2408=VECTOR('',#8368,0.25);
#2409=VECTOR('',#8381,0.25);
#2410=VECTOR('',#8394,0.25);
#2411=VECTOR('',#8399,0.15);
#2412=VECTOR('',#8404,0.15);
#2413=VECTOR('',#8409,0.15);
#2414=VECTOR('',#8414,0.15);
#2415=VECTOR('',#8425,1.);
#2416=VECTOR('',#8426,1.);
#2417=VECTOR('',#8437,1.);
#2418=VECTOR('',#8438,1.);
#2419=VECTOR('',#8443,1.);
#2420=VECTOR('',#8448,1.);
#2421=VECTOR('',#8473,0.41);
#2422=VECTOR('',#8480,0.6);
#2423=CIRCLE('',#6656,0.17);
#2424=CIRCLE('',#6657,0.17);
#2425=CIRCLE('',#6659,0.17);
#2426=CIRCLE('',#6660,0.17);
#2427=CIRCLE('',#6662,0.41);
#2428=CIRCLE('',#6663,0.41);
#2429=CIRCLE('',#6675,1.4);
#2430=CIRCLE('',#6676,1.4);
#2431=CIRCLE('',#6682,1.4);
#2432=CIRCLE('',#6684,1.4);
#2433=CIRCLE('',#6694,0.3);
#2434=CIRCLE('',#6695,0.3);
#2435=CIRCLE('',#6697,0.4);
#2436=CIRCLE('',#6699,0.4);
#2437=CIRCLE('',#6701,0.4);
#2438=CIRCLE('',#6703,0.6);
#2439=CIRCLE('',#6704,0.4);
#2440=CIRCLE('',#6706,0.6);
#2441=CIRCLE('',#6714,0.6);
#2442=CIRCLE('',#6715,0.3);
#2443=CIRCLE('',#6717,0.3);
#2444=CIRCLE('',#6719,0.6);
#2445=CIRCLE('',#6724,0.25);
#2446=CIRCLE('',#6726,0.25);
#2447=CIRCLE('',#6728,0.25);
#2448=CIRCLE('',#6730,0.25);
#2449=CIRCLE('',#6732,0.15);
#2450=CIRCLE('',#6733,0.15);
#2451=CIRCLE('',#6734,0.4);
#2452=CIRCLE('',#6736,0.15);
#2453=CIRCLE('',#6738,0.15);
#2454=CIRCLE('',#6739,0.15);
#2455=CIRCLE('',#6741,0.15);
#2456=CIRCLE('',#6742,0.15);
#2457=CIRCLE('',#6744,0.15);
#2458=CIRCLE('',#6746,0.3);
#2459=CIRCLE('',#6747,0.3);
#2460=CIRCLE('',#6749,0.17);
#2461=CIRCLE('',#6751,0.3);
#2462=CIRCLE('',#6752,0.3);
#2463=CIRCLE('',#6754,0.17);
#2464=CIRCLE('',#6756,0.17);
#2465=CIRCLE('',#6758,0.17);
#2466=CIRCLE('',#6767,0.4);
#2467=CIRCLE('',#6769,0.4);
#2468=CIRCLE('',#6783,0.4);
#2469=CIRCLE('',#6785,0.1);
#2470=CIRCLE('',#6792,0.0999999999999995);
#2471=CIRCLE('',#6794,0.1);
#2472=CIRCLE('',#6796,0.1);
#2473=CIRCLE('',#6797,0.1);
#2474=CIRCLE('',#6799,0.0999999999999999);
#2475=CIRCLE('',#6800,0.0999999999999998);
#2476=CIRCLE('',#6801,0.0999999999999998);
#2477=CIRCLE('',#6803,0.0999999999999994);
#2478=CIRCLE('',#6804,0.0999999999999993);
#2479=CIRCLE('',#6807,0.0999999999999999);
#2480=CIRCLE('',#6808,0.1);
#2481=CIRCLE('',#6812,0.3);
#2482=CIRCLE('',#6813,0.3);
#2483=CIRCLE('',#6814,0.3);
#2484=CIRCLE('',#6816,0.3);
#2485=CIRCLE('',#6817,0.3);
#2486=CIRCLE('',#6818,0.3);
#2487=CIRCLE('',#6820,0.3);
#2488=CIRCLE('',#6821,0.299999999999999);
#2489=CIRCLE('',#6822,0.3);
#2490=CIRCLE('',#6825,0.3);
#2491=CIRCLE('',#6826,0.3);
#2492=CIRCLE('',#6827,0.3);
#2493=CIRCLE('',#6834,0.25);
#2494=CIRCLE('',#6836,0.25);
#2495=CIRCLE('',#6838,0.25);
#2496=CIRCLE('',#6840,0.25);
#2497=CIRCLE('',#6842,0.15);
#2498=CIRCLE('',#6843,0.15);
#2499=CIRCLE('',#6844,0.4);
#2500=CIRCLE('',#6852,0.17);
#2501=CIRCLE('',#6860,0.17);
#2502=CIRCLE('',#6862,0.15);
#2503=CIRCLE('',#6864,0.15);
#2504=CIRCLE('',#6865,0.15);
#2505=CIRCLE('',#6867,0.15);
#2506=CIRCLE('',#6868,0.15);
#2507=CIRCLE('',#6870,0.15);
#2508=CIRCLE('',#6872,0.17);
#2509=CIRCLE('',#6874,0.17);
#2510=CIRCLE('',#6883,0.4);
#2511=CIRCLE('',#6885,0.4);
#2512=CIRCLE('',#6899,0.4);
#2513=CIRCLE('',#6901,0.1);
#2514=CIRCLE('',#6908,0.0999999999999995);
#2515=CIRCLE('',#6910,0.1);
#2516=CIRCLE('',#6912,0.1);
#2517=CIRCLE('',#6913,0.1);
#2518=CIRCLE('',#6915,0.0999999999999999);
#2519=CIRCLE('',#6916,0.0999999999999998);
#2520=CIRCLE('',#6917,0.0999999999999998);
#2521=CIRCLE('',#6919,0.0999999999999994);
#2522=CIRCLE('',#6920,0.0999999999999993);
#2523=CIRCLE('',#6923,0.0999999999999999);
#2524=CIRCLE('',#6924,0.1);
#2525=CIRCLE('',#6928,0.3);
#2526=CIRCLE('',#6929,0.3);
#2527=CIRCLE('',#6930,0.3);
#2528=CIRCLE('',#6932,0.3);
#2529=CIRCLE('',#6933,0.3);
#2530=CIRCLE('',#6934,0.3);
#2531=CIRCLE('',#6936,0.3);
#2532=CIRCLE('',#6937,0.299999999999999);
#2533=CIRCLE('',#6938,0.3);
#2534=CIRCLE('',#6941,0.3);
#2535=CIRCLE('',#6942,0.3);
#2536=CIRCLE('',#6943,0.3);
#2537=CIRCLE('',#6950,0.14635);
#2538=CIRCLE('',#6981,0.117775);
#2539=CIRCLE('',#7012,0.14635);
#2540=CIRCLE('',#7013,0.05);
#2541=CIRCLE('',#7015,0.117775);
#2542=CIRCLE('',#7025,0.275);
#2543=CIRCLE('',#7027,0.275);
#2544=CIRCLE('',#7032,0.12645);
#2545=CIRCLE('',#7034,0.12645);
#2546=CIRCLE('',#7038,0.12645);
#2547=CIRCLE('',#7040,0.1543);
#2548=CIRCLE('',#7045,0.1543);
#2549=CIRCLE('',#7058,0.35);
#2550=CIRCLE('',#7059,0.35);
#2551=CIRCLE('',#7061,0.35);
#2552=CIRCLE('',#7062,0.35);
#2553=CIRCLE('',#7064,0.25);
#2554=CIRCLE('',#7065,0.15);
#2555=CIRCLE('',#7067,0.25);
#2556=CIRCLE('',#7070,0.25);
#2557=CIRCLE('',#7071,0.15);
#2558=CIRCLE('',#7073,0.25);
#2559=CIRCLE('',#7076,0.25);
#2560=CIRCLE('',#7077,0.15);
#2561=CIRCLE('',#7079,0.25);
#2562=CIRCLE('',#7082,0.25);
#2563=CIRCLE('',#7083,0.15);
#2564=CIRCLE('',#7085,0.25);
#2565=CIRCLE('',#7088,0.15);
#2566=CIRCLE('',#7090,0.15);
#2567=CIRCLE('',#7092,0.15);
#2568=CIRCLE('',#7094,0.15);
#2569=CIRCLE('',#7095,0.0800000000000001);
#2570=CIRCLE('',#7096,0.0799999999999999);
#2571=CIRCLE('',#7098,0.0800000000000001);
#2572=CIRCLE('',#7099,0.0800000000000001);
#2573=CIRCLE('',#7100,0.0800000000000001);
#2574=CIRCLE('',#7101,0.0800000000000001);
#2575=CIRCLE('',#7103,0.0800000000000001);
#2576=CIRCLE('',#7104,0.0800000000000001);
#2577=CIRCLE('',#7119,0.41);
#2578=CIRCLE('',#7120,0.41);
#2579=CIRCLE('',#7122,0.6);
#2580=CIRCLE('',#7123,0.6);
#2581=VERTEX_POINT('',#8506);
#2582=VERTEX_POINT('',#8508);
#2583=VERTEX_POINT('',#8512);
#2584=VERTEX_POINT('',#8514);
#2585=VERTEX_POINT('',#8518);
#2586=VERTEX_POINT('',#8520);
#2587=VERTEX_POINT('',#8524);
#2588=VERTEX_POINT('',#8525);
#2589=VERTEX_POINT('',#8527);
#2590=VERTEX_POINT('',#8531);
#2591=VERTEX_POINT('',#8532);
#2592=VERTEX_POINT('',#8534);
#2593=VERTEX_POINT('',#8539);
#2594=VERTEX_POINT('',#8541);
#2595=VERTEX_POINT('',#8545);
#2596=VERTEX_POINT('',#8549);
#2597=VERTEX_POINT('',#8551);
#2598=VERTEX_POINT('',#8553);
#2599=VERTEX_POINT('',#8555);
#2600=VERTEX_POINT('',#8559);
#2601=VERTEX_POINT('',#8561);
#2602=VERTEX_POINT('',#8565);
#2603=VERTEX_POINT('',#8569);
#2604=VERTEX_POINT('',#8573);
#2605=VERTEX_POINT('',#8579);
#2606=VERTEX_POINT('',#8581);
#2607=VERTEX_POINT('',#8583);
#2608=VERTEX_POINT('',#8585);
#2609=VERTEX_POINT('',#8587);
#2610=VERTEX_POINT('',#8589);
#2611=VERTEX_POINT('',#8591);
#2612=VERTEX_POINT('',#8593);
#2613=VERTEX_POINT('',#8595);
#2614=VERTEX_POINT('',#8597);
#2615=VERTEX_POINT('',#8599);
#2616=VERTEX_POINT('',#8601);
#2617=VERTEX_POINT('',#8605);
#2618=VERTEX_POINT('',#8607);
#2619=VERTEX_POINT('',#8611);
#2620=VERTEX_POINT('',#8615);
#2621=VERTEX_POINT('',#8619);
#2622=VERTEX_POINT('',#8623);
#2623=VERTEX_POINT('',#8627);
#2624=VERTEX_POINT('',#8631);
#2625=VERTEX_POINT('',#8633);
#2626=VERTEX_POINT('',#8635);
#2627=VERTEX_POINT('',#8637);
#2628=VERTEX_POINT('',#8639);
#2629=VERTEX_POINT('',#8655);
#2630=VERTEX_POINT('',#8657);
#2631=VERTEX_POINT('',#8661);
#2632=VERTEX_POINT('',#8664);
#2633=VERTEX_POINT('',#8667);
#2634=VERTEX_POINT('',#8671);
#2635=VERTEX_POINT('',#8673);
#2636=VERTEX_POINT('',#8676);
#2637=VERTEX_POINT('',#8685);
#2638=VERTEX_POINT('',#8686);
#2639=VERTEX_POINT('',#8688);
#2640=VERTEX_POINT('',#8690);
#2641=VERTEX_POINT('',#8694);
#2642=VERTEX_POINT('',#8695);
#2643=VERTEX_POINT('',#8697);
#2644=VERTEX_POINT('',#8699);
#2645=VERTEX_POINT('',#8713);
#2646=VERTEX_POINT('',#8714);
#2647=VERTEX_POINT('',#8741);
#2648=VERTEX_POINT('',#8742);
#2649=VERTEX_POINT('',#8765);
#2650=VERTEX_POINT('',#8766);
#2651=VERTEX_POINT('',#8789);
#2652=VERTEX_POINT('',#8790);
#2653=VERTEX_POINT('',#8836);
#2654=VERTEX_POINT('',#8841);
#2655=VERTEX_POINT('',#8870);
#2656=VERTEX_POINT('',#8875);
#2657=VERTEX_POINT('',#8928);
#2658=VERTEX_POINT('',#8933);
#2659=VERTEX_POINT('',#8962);
#2660=VERTEX_POINT('',#8967);
#2661=VERTEX_POINT('',#9001);
#2662=VERTEX_POINT('',#9007);
#2663=VERTEX_POINT('',#9013);
#2664=VERTEX_POINT('',#9015);
#2665=VERTEX_POINT('',#9017);
#2666=VERTEX_POINT('',#9020);
#2667=VERTEX_POINT('',#9024);
#2668=VERTEX_POINT('',#9026);
#2669=VERTEX_POINT('',#9030);
#2670=VERTEX_POINT('',#9032);
#2671=VERTEX_POINT('',#9036);
#2672=VERTEX_POINT('',#9040);
#2673=VERTEX_POINT('',#9042);
#2674=VERTEX_POINT('',#9046);
#2675=VERTEX_POINT('',#9049);
#2676=VERTEX_POINT('',#9051);
#2677=VERTEX_POINT('',#9055);
#2678=VERTEX_POINT('',#9058);
#2679=VERTEX_POINT('',#9062);
#2680=VERTEX_POINT('',#9066);
#2681=VERTEX_POINT('',#9067);
#2682=VERTEX_POINT('',#9069);
#2683=VERTEX_POINT('',#9071);
#2684=VERTEX_POINT('',#9075);
#2685=VERTEX_POINT('',#9076);
#2686=VERTEX_POINT('',#9078);
#2687=VERTEX_POINT('',#9080);
#2688=VERTEX_POINT('',#9084);
#2689=VERTEX_POINT('',#9085);
#2690=VERTEX_POINT('',#9087);
#2691=VERTEX_POINT('',#9089);
#2692=VERTEX_POINT('',#9093);
#2693=VERTEX_POINT('',#9094);
#2694=VERTEX_POINT('',#9096);
#2695=VERTEX_POINT('',#9098);
#2696=VERTEX_POINT('',#9102);
#2697=VERTEX_POINT('',#9103);
#2698=VERTEX_POINT('',#9105);
#2699=VERTEX_POINT('',#9107);
#2700=VERTEX_POINT('',#9111);
#2701=VERTEX_POINT('',#9112);
#2702=VERTEX_POINT('',#9114);
#2703=VERTEX_POINT('',#9116);
#2704=VERTEX_POINT('',#9120);
#2705=VERTEX_POINT('',#9121);
#2706=VERTEX_POINT('',#9123);
#2707=VERTEX_POINT('',#9125);
#2708=VERTEX_POINT('',#9129);
#2709=VERTEX_POINT('',#9132);
#2710=VERTEX_POINT('',#9144);
#2711=VERTEX_POINT('',#9146);
#2712=VERTEX_POINT('',#9150);
#2713=VERTEX_POINT('',#9152);
#2714=VERTEX_POINT('',#9156);
#2715=VERTEX_POINT('',#9157);
#2716=VERTEX_POINT('',#9159);
#2717=VERTEX_POINT('',#9201);
#2718=VERTEX_POINT('',#9209);
#2719=VERTEX_POINT('',#9238);
#2720=VERTEX_POINT('',#9247);
#2721=VERTEX_POINT('',#9249);
#2722=VERTEX_POINT('',#9256);
#2723=VERTEX_POINT('',#9285);
#2724=VERTEX_POINT('',#9287);
#2725=VERTEX_POINT('',#9316);
#2726=VERTEX_POINT('',#9325);
#2727=VERTEX_POINT('',#9333);
#2728=VERTEX_POINT('',#9335);
#2729=VERTEX_POINT('',#9364);
#2730=VERTEX_POINT('',#9373);
#2731=VERTEX_POINT('',#9375);
#2732=VERTEX_POINT('',#9380);
#2733=VERTEX_POINT('',#9382);
#2734=VERTEX_POINT('',#9397);
#2735=VERTEX_POINT('',#9406);
#2736=VERTEX_POINT('',#9412);
#2737=VERTEX_POINT('',#9414);
#2738=VERTEX_POINT('',#9447);
#2739=VERTEX_POINT('',#9449);
#2740=VERTEX_POINT('',#9481);
#2741=VERTEX_POINT('',#9486);
#2742=VERTEX_POINT('',#9518);
#2743=VERTEX_POINT('',#9520);
#2744=VERTEX_POINT('',#9552);
#2745=VERTEX_POINT('',#9557);
#2746=VERTEX_POINT('',#9590);
#2747=VERTEX_POINT('',#9616);
#2748=VERTEX_POINT('',#9622);
#2749=VERTEX_POINT('',#9628);
#2750=VERTEX_POINT('',#9637);
#2751=VERTEX_POINT('',#9638);
#2752=VERTEX_POINT('',#9643);
#2753=VERTEX_POINT('',#9672);
#2754=VERTEX_POINT('',#9674);
#2755=VERTEX_POINT('',#9703);
#2756=VERTEX_POINT('',#9712);
#2757=VERTEX_POINT('',#9716);
#2758=VERTEX_POINT('',#9723);
#2759=VERTEX_POINT('',#9730);
#2760=VERTEX_POINT('',#9759);
#2761=VERTEX_POINT('',#9825);
#2762=VERTEX_POINT('',#9874);
#2763=VERTEX_POINT('',#9881);
#2764=VERTEX_POINT('',#9919);
#2765=VERTEX_POINT('',#9929);
#2766=VERTEX_POINT('',#9936);
#2767=VERTEX_POINT('',#9965);
#2768=VERTEX_POINT('',#9967);
#2769=VERTEX_POINT('',#10092);
#2770=VERTEX_POINT('',#10099);
#2771=VERTEX_POINT('',#10201);
#2772=VERTEX_POINT('',#10208);
#2773=VERTEX_POINT('',#10237);
#2774=VERTEX_POINT('',#10239);
#2775=VERTEX_POINT('',#10290);
#2776=VERTEX_POINT('',#10319);
#2777=VERTEX_POINT('',#10326);
#2778=VERTEX_POINT('',#10348);
#2779=VERTEX_POINT('',#10383);
#2780=VERTEX_POINT('',#10411);
#2781=VERTEX_POINT('',#10506);
#2782=VERTEX_POINT('',#10507);
#2783=VERTEX_POINT('',#10509);
#2784=VERTEX_POINT('',#10513);
#2785=VERTEX_POINT('',#10514);
#2786=VERTEX_POINT('',#10516);
#2787=VERTEX_POINT('',#10520);
#2788=VERTEX_POINT('',#10521);
#2789=VERTEX_POINT('',#10523);
#2790=VERTEX_POINT('',#10558);
#2791=VERTEX_POINT('',#10559);
#2792=VERTEX_POINT('',#10561);
#2793=VERTEX_POINT('',#10758);
#2794=VERTEX_POINT('',#10759);
#2795=VERTEX_POINT('',#10786);
#2796=VERTEX_POINT('',#10787);
#2797=VERTEX_POINT('',#10810);
#2798=VERTEX_POINT('',#10811);
#2799=VERTEX_POINT('',#10834);
#2800=VERTEX_POINT('',#10835);
#2801=VERTEX_POINT('',#10881);
#2802=VERTEX_POINT('',#10886);
#2803=VERTEX_POINT('',#10915);
#2804=VERTEX_POINT('',#10920);
#2805=VERTEX_POINT('',#10973);
#2806=VERTEX_POINT('',#10978);
#2807=VERTEX_POINT('',#11007);
#2808=VERTEX_POINT('',#11012);
#2809=VERTEX_POINT('',#11046);
#2810=VERTEX_POINT('',#11052);
#2811=VERTEX_POINT('',#11058);
#2812=VERTEX_POINT('',#11060);
#2813=VERTEX_POINT('',#11062);
#2814=VERTEX_POINT('',#11065);
#2815=VERTEX_POINT('',#11066);
#2816=VERTEX_POINT('',#11068);
#2817=VERTEX_POINT('',#11070);
#2818=VERTEX_POINT('',#11074);
#2819=VERTEX_POINT('',#11076);
#2820=VERTEX_POINT('',#11080);
#2821=VERTEX_POINT('',#11082);
#2822=VERTEX_POINT('',#11086);
#2823=VERTEX_POINT('',#11088);
#2824=VERTEX_POINT('',#11092);
#2825=VERTEX_POINT('',#11094);
#2826=VERTEX_POINT('',#11101);
#2827=VERTEX_POINT('',#11104);
#2828=VERTEX_POINT('',#11105);
#2829=VERTEX_POINT('',#11107);
#2830=VERTEX_POINT('',#11109);
#2831=VERTEX_POINT('',#11113);
#2832=VERTEX_POINT('',#11115);
#2833=VERTEX_POINT('',#11119);
#2834=VERTEX_POINT('',#11121);
#2835=VERTEX_POINT('',#11125);
#2836=VERTEX_POINT('',#11127);
#2837=VERTEX_POINT('',#11131);
#2838=VERTEX_POINT('',#11133);
#2839=VERTEX_POINT('',#11140);
#2840=VERTEX_POINT('',#11143);
#2841=VERTEX_POINT('',#11147);
#2842=VERTEX_POINT('',#11149);
#2843=VERTEX_POINT('',#11153);
#2844=VERTEX_POINT('',#11155);
#2845=VERTEX_POINT('',#11159);
#2846=VERTEX_POINT('',#11163);
#2847=VERTEX_POINT('',#11167);
#2848=VERTEX_POINT('',#11171);
#2849=VERTEX_POINT('',#11172);
#2850=VERTEX_POINT('',#11174);
#2851=VERTEX_POINT('',#11176);
#2852=VERTEX_POINT('',#11180);
#2853=VERTEX_POINT('',#11181);
#2854=VERTEX_POINT('',#11183);
#2855=VERTEX_POINT('',#11185);
#2856=VERTEX_POINT('',#11189);
#2857=VERTEX_POINT('',#11190);
#2858=VERTEX_POINT('',#11192);
#2859=VERTEX_POINT('',#11194);
#2860=VERTEX_POINT('',#11198);
#2861=VERTEX_POINT('',#11199);
#2862=VERTEX_POINT('',#11201);
#2863=VERTEX_POINT('',#11203);
#2864=VERTEX_POINT('',#11207);
#2865=VERTEX_POINT('',#11208);
#2866=VERTEX_POINT('',#11210);
#2867=VERTEX_POINT('',#11212);
#2868=VERTEX_POINT('',#11216);
#2869=VERTEX_POINT('',#11217);
#2870=VERTEX_POINT('',#11219);
#2871=VERTEX_POINT('',#11221);
#2872=VERTEX_POINT('',#11225);
#2873=VERTEX_POINT('',#11226);
#2874=VERTEX_POINT('',#11228);
#2875=VERTEX_POINT('',#11230);
#2876=VERTEX_POINT('',#11234);
#2877=VERTEX_POINT('',#11237);
#2878=VERTEX_POINT('',#11249);
#2879=VERTEX_POINT('',#11251);
#2880=VERTEX_POINT('',#11255);
#2881=VERTEX_POINT('',#11257);
#2882=VERTEX_POINT('',#11261);
#2883=VERTEX_POINT('',#11262);
#2884=VERTEX_POINT('',#11264);
#2885=VERTEX_POINT('',#11306);
#2886=VERTEX_POINT('',#11314);
#2887=VERTEX_POINT('',#11343);
#2888=VERTEX_POINT('',#11352);
#2889=VERTEX_POINT('',#11354);
#2890=VERTEX_POINT('',#11361);
#2891=VERTEX_POINT('',#11390);
#2892=VERTEX_POINT('',#11392);
#2893=VERTEX_POINT('',#11421);
#2894=VERTEX_POINT('',#11430);
#2895=VERTEX_POINT('',#11438);
#2896=VERTEX_POINT('',#11440);
#2897=VERTEX_POINT('',#11469);
#2898=VERTEX_POINT('',#11478);
#2899=VERTEX_POINT('',#11480);
#2900=VERTEX_POINT('',#11485);
#2901=VERTEX_POINT('',#11487);
#2902=VERTEX_POINT('',#11502);
#2903=VERTEX_POINT('',#11511);
#2904=VERTEX_POINT('',#11517);
#2905=VERTEX_POINT('',#11519);
#2906=VERTEX_POINT('',#11552);
#2907=VERTEX_POINT('',#11554);
#2908=VERTEX_POINT('',#11586);
#2909=VERTEX_POINT('',#11591);
#2910=VERTEX_POINT('',#11623);
#2911=VERTEX_POINT('',#11625);
#2912=VERTEX_POINT('',#11657);
#2913=VERTEX_POINT('',#11662);
#2914=VERTEX_POINT('',#11695);
#2915=VERTEX_POINT('',#11721);
#2916=VERTEX_POINT('',#11727);
#2917=VERTEX_POINT('',#11733);
#2918=VERTEX_POINT('',#11742);
#2919=VERTEX_POINT('',#11743);
#2920=VERTEX_POINT('',#11748);
#2921=VERTEX_POINT('',#11777);
#2922=VERTEX_POINT('',#11779);
#2923=VERTEX_POINT('',#11808);
#2924=VERTEX_POINT('',#11817);
#2925=VERTEX_POINT('',#11821);
#2926=VERTEX_POINT('',#11828);
#2927=VERTEX_POINT('',#11835);
#2928=VERTEX_POINT('',#11864);
#2929=VERTEX_POINT('',#11930);
#2930=VERTEX_POINT('',#11979);
#2931=VERTEX_POINT('',#11986);
#2932=VERTEX_POINT('',#12024);
#2933=VERTEX_POINT('',#12034);
#2934=VERTEX_POINT('',#12041);
#2935=VERTEX_POINT('',#12070);
#2936=VERTEX_POINT('',#12072);
#2937=VERTEX_POINT('',#12197);
#2938=VERTEX_POINT('',#12204);
#2939=VERTEX_POINT('',#12306);
#2940=VERTEX_POINT('',#12313);
#2941=VERTEX_POINT('',#12342);
#2942=VERTEX_POINT('',#12344);
#2943=VERTEX_POINT('',#12395);
#2944=VERTEX_POINT('',#12424);
#2945=VERTEX_POINT('',#12431);
#2946=VERTEX_POINT('',#12453);
#2947=VERTEX_POINT('',#12488);
#2948=VERTEX_POINT('',#12516);
#2949=VERTEX_POINT('',#12611);
#2950=VERTEX_POINT('',#12612);
#2951=VERTEX_POINT('',#12614);
#2952=VERTEX_POINT('',#12618);
#2953=VERTEX_POINT('',#12619);
#2954=VERTEX_POINT('',#12621);
#2955=VERTEX_POINT('',#12625);
#2956=VERTEX_POINT('',#12626);
#2957=VERTEX_POINT('',#12628);
#2958=VERTEX_POINT('',#12663);
#2959=VERTEX_POINT('',#12664);
#2960=VERTEX_POINT('',#12666);
#2961=VERTEX_POINT('',#12863);
#2962=VERTEX_POINT('',#12864);
#2963=VERTEX_POINT('',#12866);
#2964=VERTEX_POINT('',#12877);
#2965=VERTEX_POINT('',#12887);
#2966=VERTEX_POINT('',#12888);
#2967=VERTEX_POINT('',#12935);
#2968=VERTEX_POINT('',#12936);
#2969=VERTEX_POINT('',#12983);
#2970=VERTEX_POINT('',#12984);
#2971=VERTEX_POINT('',#13034);
#2972=VERTEX_POINT('',#13035);
#2973=VERTEX_POINT('',#13082);
#2974=VERTEX_POINT('',#13083);
#2975=VERTEX_POINT('',#13130);
#2976=VERTEX_POINT('',#13131);
#2977=VERTEX_POINT('',#13178);
#2978=VERTEX_POINT('',#13179);
#2979=VERTEX_POINT('',#13232);
#2980=VERTEX_POINT('',#13233);
#2981=VERTEX_POINT('',#13280);
#2982=VERTEX_POINT('',#13281);
#2983=VERTEX_POINT('',#13328);
#2984=VERTEX_POINT('',#13329);
#2985=VERTEX_POINT('',#13382);
#2986=VERTEX_POINT('',#13383);
#2987=VERTEX_POINT('',#13430);
#2988=VERTEX_POINT('',#13431);
#2989=VERTEX_POINT('',#13478);
#2990=VERTEX_POINT('',#13479);
#2991=VERTEX_POINT('',#13526);
#2992=VERTEX_POINT('',#13527);
#2993=VERTEX_POINT('',#13580);
#2994=VERTEX_POINT('',#13581);
#2995=VERTEX_POINT('',#13628);
#2996=VERTEX_POINT('',#13629);
#2997=VERTEX_POINT('',#13676);
#2998=VERTEX_POINT('',#13677);
#2999=VERTEX_POINT('',#13730);
#3000=VERTEX_POINT('',#13731);
#3001=VERTEX_POINT('',#13778);
#3002=VERTEX_POINT('',#13779);
#3003=VERTEX_POINT('',#13826);
#3004=VERTEX_POINT('',#13827);
#3005=VERTEX_POINT('',#13880);
#3006=VERTEX_POINT('',#13881);
#3007=VERTEX_POINT('',#13928);
#3008=VERTEX_POINT('',#13929);
#3009=VERTEX_POINT('',#13976);
#3010=VERTEX_POINT('',#13977);
#3011=VERTEX_POINT('',#14024);
#3012=VERTEX_POINT('',#14025);
#3013=VERTEX_POINT('',#14078);
#3014=VERTEX_POINT('',#14079);
#3015=VERTEX_POINT('',#14126);
#3016=VERTEX_POINT('',#14127);
#3017=VERTEX_POINT('',#14174);
#3018=VERTEX_POINT('',#14175);
#3019=VERTEX_POINT('',#14228);
#3020=VERTEX_POINT('',#14229);
#3021=VERTEX_POINT('',#14276);
#3022=VERTEX_POINT('',#14277);
#3023=VERTEX_POINT('',#14324);
#3024=VERTEX_POINT('',#14325);
#3025=VERTEX_POINT('',#14327);
#3026=VERTEX_POINT('',#14338);
#3027=VERTEX_POINT('',#14350);
#3028=VERTEX_POINT('',#14351);
#3029=VERTEX_POINT('',#14374);
#3030=VERTEX_POINT('',#14375);
#3031=VERTEX_POINT('',#14398);
#3032=VERTEX_POINT('',#14399);
#3033=VERTEX_POINT('',#14423);
#3034=VERTEX_POINT('',#14424);
#3035=VERTEX_POINT('',#14448);
#3036=VERTEX_POINT('',#14449);
#3037=VERTEX_POINT('',#14472);
#3038=VERTEX_POINT('',#14473);
#3039=VERTEX_POINT('',#14497);
#3040=VERTEX_POINT('',#14498);
#3041=VERTEX_POINT('',#14522);
#3042=VERTEX_POINT('',#14523);
#3043=VERTEX_POINT('',#14546);
#3044=VERTEX_POINT('',#14547);
#3045=VERTEX_POINT('',#14570);
#3046=VERTEX_POINT('',#14571);
#3047=VERTEX_POINT('',#14595);
#3048=VERTEX_POINT('',#14596);
#3049=VERTEX_POINT('',#14620);
#3050=VERTEX_POINT('',#14621);
#3051=VERTEX_POINT('',#14644);
#3052=VERTEX_POINT('',#14645);
#3053=VERTEX_POINT('',#14669);
#3054=VERTEX_POINT('',#14670);
#3055=VERTEX_POINT('',#14694);
#3056=VERTEX_POINT('',#14695);
#3057=VERTEX_POINT('',#14718);
#3058=VERTEX_POINT('',#14719);
#3059=VERTEX_POINT('',#14743);
#3060=VERTEX_POINT('',#14744);
#3061=VERTEX_POINT('',#14768);
#3062=VERTEX_POINT('',#14769);
#3063=VERTEX_POINT('',#14792);
#3064=VERTEX_POINT('',#14793);
#3065=VERTEX_POINT('',#14816);
#3066=VERTEX_POINT('',#14817);
#3067=VERTEX_POINT('',#14841);
#3068=VERTEX_POINT('',#14842);
#3069=VERTEX_POINT('',#14866);
#3070=VERTEX_POINT('',#14867);
#3071=VERTEX_POINT('',#14890);
#3072=VERTEX_POINT('',#14891);
#3073=VERTEX_POINT('',#14915);
#3074=VERTEX_POINT('',#14916);
#3075=VERTEX_POINT('',#14940);
#3076=VERTEX_POINT('',#14941);
#3077=VERTEX_POINT('',#14964);
#3078=VERTEX_POINT('',#14965);
#3079=VERTEX_POINT('',#14989);
#3080=VERTEX_POINT('',#14990);
#3081=VERTEX_POINT('',#15013);
#3082=VERTEX_POINT('',#15014);
#3083=VERTEX_POINT('',#15038);
#3084=VERTEX_POINT('',#15039);
#3085=VERTEX_POINT('',#15062);
#3086=VERTEX_POINT('',#15184);
#3087=VERTEX_POINT('',#15222);
#3088=VERTEX_POINT('',#15240);
#3089=VERTEX_POINT('',#16027);
#3090=VERTEX_POINT('',#16105);
#3091=VERTEX_POINT('',#16984);
#3092=VERTEX_POINT('',#16985);
#3093=VERTEX_POINT('',#16987);
#3094=VERTEX_POINT('',#16989);
#3095=VERTEX_POINT('',#16993);
#3096=VERTEX_POINT('',#16995);
#3097=VERTEX_POINT('',#16999);
#3098=VERTEX_POINT('',#17001);
#3099=VERTEX_POINT('',#17005);
#3100=VERTEX_POINT('',#17007);
#3101=VERTEX_POINT('',#17011);
#3102=VERTEX_POINT('',#17013);
#3103=VERTEX_POINT('',#17021);
#3104=VERTEX_POINT('',#17024);
#3105=VERTEX_POINT('',#17031);
#3106=VERTEX_POINT('',#17032);
#3107=VERTEX_POINT('',#17034);
#3108=VERTEX_POINT('',#17044);
#3109=VERTEX_POINT('',#17045);
#3110=VERTEX_POINT('',#17047);
#3111=VERTEX_POINT('',#17091);
#3112=VERTEX_POINT('',#17092);
#3113=VERTEX_POINT('',#17145);
#3114=VERTEX_POINT('',#17146);
#3115=VERTEX_POINT('',#17193);
#3116=VERTEX_POINT('',#17194);
#3117=VERTEX_POINT('',#17196);
#3118=VERTEX_POINT('',#17210);
#3119=VERTEX_POINT('',#17232);
#3120=VERTEX_POINT('',#17233);
#3121=VERTEX_POINT('',#17235);
#3122=VERTEX_POINT('',#17243);
#3123=VERTEX_POINT('',#17253);
#3124=VERTEX_POINT('',#17254);
#3125=VERTEX_POINT('',#17278);
#3126=VERTEX_POINT('',#17279);
#3127=VERTEX_POINT('',#17303);
#3128=VERTEX_POINT('',#17304);
#3129=VERTEX_POINT('',#17328);
#3130=VERTEX_POINT('',#17329);
#3131=VERTEX_POINT('',#17331);
#3132=VERTEX_POINT('',#17337);
#3133=VERTEX_POINT('',#17901);
#3134=VERTEX_POINT('',#17902);
#3135=VERTEX_POINT('',#17904);
#3136=VERTEX_POINT('',#17906);
#3137=VERTEX_POINT('',#17908);
#3138=VERTEX_POINT('',#17910);
#3139=VERTEX_POINT('',#17915);
#3140=VERTEX_POINT('',#17916);
#3141=VERTEX_POINT('',#17921);
#3142=VERTEX_POINT('',#17925);
#3143=VERTEX_POINT('',#17929);
#3144=VERTEX_POINT('',#17933);
#3145=VERTEX_POINT('',#17941);
#3146=VERTEX_POINT('',#17943);
#3147=VERTEX_POINT('',#17947);
#3148=VERTEX_POINT('',#17949);
#3149=VERTEX_POINT('',#17953);
#3150=VERTEX_POINT('',#17955);
#3151=VERTEX_POINT('',#17958);
#3152=VERTEX_POINT('',#17963);
#3153=VERTEX_POINT('',#17965);
#3154=VERTEX_POINT('',#17968);
#3155=VERTEX_POINT('',#17973);
#3156=VERTEX_POINT('',#17975);
#3157=VERTEX_POINT('',#17978);
#3158=VERTEX_POINT('',#17983);
#3159=VERTEX_POINT('',#17985);
#3160=VERTEX_POINT('',#17988);
#3161=VERTEX_POINT('',#17993);
#3162=VERTEX_POINT('',#17997);
#3163=VERTEX_POINT('',#18001);
#3164=VERTEX_POINT('',#18005);
#3165=VERTEX_POINT('',#18033);
#3166=VERTEX_POINT('',#18034);
#3167=VERTEX_POINT('',#18036);
#3168=VERTEX_POINT('',#18042);
#3169=VERTEX_POINT('',#18050);
#3170=VERTEX_POINT('',#18051);
#3171=VERTEX_POINT('',#18080);
#3172=VERTEX_POINT('',#18081);
#3173=VERTEX_POINT('',#18118);
#3174=VERTEX_POINT('',#18119);
#3175=VERTEX_POINT('',#18156);
#3176=VERTEX_POINT('',#18157);
#3177=VERTEX_POINT('',#18170);
#3178=VERTEX_POINT('',#18171);
#3179=VERTEX_POINT('',#18200);
#3180=VERTEX_POINT('',#18201);
#3181=VERTEX_POINT('',#18249);
#3182=VERTEX_POINT('',#18254);
#3183=VERTEX_POINT('',#18280);
#3184=VERTEX_POINT('',#18329);
#3185=VERTEX_POINT('',#18358);
#3186=VERTEX_POINT('',#18393);
#3187=VERTEX_POINT('',#18419);
#3188=VERTEX_POINT('',#18472);
#3189=VERTEX_POINT('',#18536);
#3190=VERTEX_POINT('',#18538);
#3191=VERTEX_POINT('',#18542);
#3192=VERTEX_POINT('',#18544);
#3193=EDGE_CURVE('',#2581,#2581,#2423,.T.);
#3194=EDGE_CURVE('',#2581,#2582,#1609,.T.);
#3195=EDGE_CURVE('',#2582,#2582,#2424,.T.);
#3196=EDGE_CURVE('',#2583,#2583,#2425,.T.);
#3197=EDGE_CURVE('',#2583,#2584,#1610,.T.);
#3198=EDGE_CURVE('',#2584,#2584,#2426,.T.);
#3199=EDGE_CURVE('',#2585,#2585,#2427,.T.);
#3200=EDGE_CURVE('',#2585,#2586,#1611,.T.);
#3201=EDGE_CURVE('',#2586,#2586,#2428,.T.);
#3202=EDGE_CURVE('',#2587,#2588,#1612,.T.);
#3203=EDGE_CURVE('',#2589,#2587,#1613,.T.);
#3204=EDGE_CURVE('',#2589,#2588,#1614,.T.);
#3205=EDGE_CURVE('',#2590,#2591,#1615,.T.);
#3206=EDGE_CURVE('',#2592,#2590,#1616,.T.);
#3207=EDGE_CURVE('',#2589,#2592,#1617,.T.);
#3208=EDGE_CURVE('',#2591,#2587,#1618,.T.);
#3209=EDGE_CURVE('',#2593,#2590,#1619,.T.);
#3210=EDGE_CURVE('',#2594,#2593,#1620,.T.);
#3211=EDGE_CURVE('',#2592,#2594,#1621,.T.);
#3212=EDGE_CURVE('',#2593,#2595,#1622,.T.);
#3213=EDGE_CURVE('',#2595,#2594,#1623,.T.);
#3214=EDGE_CURVE('',#2588,#2596,#1624,.T.);
#3215=EDGE_CURVE('',#2597,#2596,#1625,.T.);
#3216=EDGE_CURVE('',#2597,#2598,#1626,.T.);
#3217=EDGE_CURVE('',#2598,#2599,#1627,.T.);
#3218=EDGE_CURVE('',#2599,#2591,#1628,.T.);
#3219=EDGE_CURVE('',#2600,#2597,#1629,.T.);
#3220=EDGE_CURVE('',#2601,#2600,#1630,.T.);
#3221=EDGE_CURVE('',#2601,#2598,#1631,.T.);
#3222=EDGE_CURVE('',#2596,#2602,#1632,.T.);
#3223=EDGE_CURVE('',#2602,#2589,#1633,.T.);
#3224=EDGE_CURVE('',#2592,#2603,#1634,.T.);
#3225=EDGE_CURVE('',#2603,#2595,#1635,.T.);
#3226=EDGE_CURVE('',#2604,#2599,#1636,.T.);
#3227=EDGE_CURVE('',#2603,#2604,#1637,.T.);
#3228=EDGE_CURVE('',#2604,#2601,#1638,.T.);
#3229=EDGE_CURVE('',#2600,#2605,#1639,.T.);
#3230=EDGE_CURVE('',#2605,#2606,#1640,.T.);
#3231=EDGE_CURVE('',#2606,#2607,#1641,.T.);
#3232=EDGE_CURVE('',#2608,#2607,#2429,.T.);
#3233=EDGE_CURVE('',#2609,#2608,#1642,.T.);
#3234=EDGE_CURVE('',#2610,#2609,#1643,.T.);
#3235=EDGE_CURVE('',#2611,#2610,#1644,.T.);
#3236=EDGE_CURVE('',#2612,#2611,#1645,.T.);
#3237=EDGE_CURVE('',#2613,#2612,#1646,.T.);
#3238=EDGE_CURVE('',#2614,#2613,#1647,.T.);
#3239=EDGE_CURVE('',#2615,#2614,#2430,.T.);
#3240=EDGE_CURVE('',#2615,#2616,#1648,.T.);
#3241=EDGE_CURVE('',#2616,#2602,#1649,.T.);
#3242=EDGE_CURVE('',#2617,#2615,#1650,.T.);
#3243=EDGE_CURVE('',#2618,#2617,#1651,.T.);
#3244=EDGE_CURVE('',#2616,#2618,#1652,.T.);
#3245=EDGE_CURVE('',#2619,#2618,#1653,.T.);
#3246=EDGE_CURVE('',#2605,#2619,#1654,.T.);
#3247=EDGE_CURVE('',#2620,#2619,#1655,.T.);
#3248=EDGE_CURVE('',#2606,#2620,#1656,.T.);
#3249=EDGE_CURVE('',#2607,#2621,#1657,.T.);
#3250=EDGE_CURVE('',#2621,#2620,#1658,.T.);
#3251=EDGE_CURVE('',#2614,#2622,#1659,.T.);
#3252=EDGE_CURVE('',#2617,#2622,#2431,.T.);
#3253=EDGE_CURVE('',#2623,#2621,#2432,.T.);
#3254=EDGE_CURVE('',#2623,#2608,#1660,.T.);
#3255=EDGE_CURVE('',#2622,#2624,#1661,.T.);
#3256=EDGE_CURVE('',#2624,#2625,#1662,.T.);
#3257=EDGE_CURVE('',#2625,#2626,#1663,.T.);
#3258=EDGE_CURVE('',#2626,#2627,#1664,.T.);
#3259=EDGE_CURVE('',#2627,#2628,#1665,.T.);
#3260=EDGE_CURVE('',#2628,#2623,#1666,.T.);
#3261=EDGE_CURVE('',#2613,#2624,#1667,.T.);
#3262=EDGE_CURVE('',#2609,#2628,#1668,.T.);
#3263=EDGE_CURVE('',#2610,#2627,#1669,.T.);
#3264=EDGE_CURVE('',#2611,#2626,#1670,.T.);
#3265=EDGE_CURVE('',#2612,#2625,#1671,.T.);
#3266=EDGE_CURVE('',#2629,#2629,#2433,.T.);
#3267=EDGE_CURVE('',#2629,#2630,#1672,.T.);
#3268=EDGE_CURVE('',#2630,#2630,#2434,.T.);
#3269=EDGE_CURVE('',#2631,#2631,#2435,.T.);
#3270=EDGE_CURVE('',#2632,#2632,#2436,.T.);
#3271=EDGE_CURVE('',#2633,#2633,#2437,.T.);
#3272=EDGE_CURVE('',#2633,#2632,#1673,.T.);
#3273=EDGE_CURVE('',#2634,#2634,#2438,.T.);
#3274=EDGE_CURVE('',#2635,#2635,#2439,.T.);
#3275=EDGE_CURVE('',#2634,#2636,#1674,.T.);
#3276=EDGE_CURVE('',#2636,#2636,#2440,.T.);
#3277=EDGE_CURVE('',#2631,#2635,#1675,.T.);
#3278=EDGE_CURVE('',#2637,#2638,#1676,.T.);
#3279=EDGE_CURVE('',#2639,#2637,#1677,.T.);
#3280=EDGE_CURVE('',#2640,#2639,#1678,.T.);
#3281=EDGE_CURVE('',#2638,#2640,#1679,.T.);
#3282=EDGE_CURVE('',#2641,#2642,#1680,.T.);
#3283=EDGE_CURVE('',#2643,#2641,#1681,.T.);
#3284=EDGE_CURVE('',#2644,#2643,#1682,.T.);
#3285=EDGE_CURVE('',#2642,#2644,#1683,.T.);
#3286=EDGE_CURVE('',#2639,#2644,#2441,.T.);
#3287=EDGE_CURVE('',#2642,#2637,#2442,.T.);
#3288=EDGE_CURVE('',#2641,#2638,#2443,.T.);
#3289=EDGE_CURVE('',#2640,#2643,#2444,.T.);
#3290=EDGE_CURVE('',#2645,#2646,#172,.T.);
#3291=EDGE_CURVE('',#2645,#2646,#2445,.T.);
#3292=EDGE_CURVE('',#2647,#2648,#173,.T.);
#3293=EDGE_CURVE('',#2647,#2648,#2446,.T.);
#3294=EDGE_CURVE('',#2649,#2650,#174,.T.);
#3295=EDGE_CURVE('',#2649,#2650,#2447,.T.);
#3296=EDGE_CURVE('',#2651,#2652,#175,.T.);
#3297=EDGE_CURVE('',#2651,#2652,#2448,.T.);
#3298=EDGE_CURVE('',#2653,#2648,#176,.T.);
#3299=EDGE_CURVE('',#2653,#2654,#177,.T.);
#3300=EDGE_CURVE('',#2655,#2654,#178,.T.);
#3301=EDGE_CURVE('',#2655,#2656,#179,.T.);
#3302=EDGE_CURVE('',#2647,#2656,#180,.T.);
#3303=EDGE_CURVE('',#2657,#2652,#181,.T.);
#3304=EDGE_CURVE('',#2657,#2658,#182,.T.);
#3305=EDGE_CURVE('',#2659,#2658,#183,.T.);
#3306=EDGE_CURVE('',#2659,#2660,#184,.T.);
#3307=EDGE_CURVE('',#2651,#2660,#185,.T.);
#3308=EDGE_CURVE('',#2645,#2661,#186,.T.);
#3309=EDGE_CURVE('',#2661,#2657,#1684,.T.);
#3310=EDGE_CURVE('',#2660,#2662,#1685,.T.);
#3311=EDGE_CURVE('',#2662,#2646,#187,.T.);
#3312=EDGE_CURVE('',#2663,#2663,#2449,.T.);
#3313=EDGE_CURVE('',#2664,#2664,#2450,.T.);
#3314=EDGE_CURVE('',#2665,#2665,#2451,.T.);
#3315=EDGE_CURVE('',#2666,#2666,#2452,.T.);
#3316=EDGE_CURVE('',#2666,#2663,#1686,.T.);
#3317=EDGE_CURVE('',#2667,#2667,#2453,.T.);
#3318=EDGE_CURVE('',#2667,#2668,#1687,.T.);
#3319=EDGE_CURVE('',#2668,#2668,#2454,.T.);
#3320=EDGE_CURVE('',#2669,#2669,#2455,.T.);
#3321=EDGE_CURVE('',#2669,#2670,#1688,.T.);
#3322=EDGE_CURVE('',#2670,#2670,#2456,.T.);
#3323=EDGE_CURVE('',#2671,#2671,#2457,.T.);
#3324=EDGE_CURVE('',#2671,#2664,#1689,.T.);
#3325=EDGE_CURVE('',#2672,#2672,#2458,.T.);
#3326=EDGE_CURVE('',#2672,#2673,#1690,.T.);
#3327=EDGE_CURVE('',#2673,#2673,#2459,.T.);
#3328=EDGE_CURVE('',#2674,#2674,#2460,.T.);
#3329=EDGE_CURVE('',#2675,#2675,#2461,.T.);
#3330=EDGE_CURVE('',#2675,#2676,#1691,.T.);
#3331=EDGE_CURVE('',#2676,#2676,#2462,.T.);
#3332=EDGE_CURVE('',#2677,#2677,#2463,.T.);
#3333=EDGE_CURVE('',#2674,#2678,#1692,.T.);
#3334=EDGE_CURVE('',#2678,#2678,#2464,.T.);
#3335=EDGE_CURVE('',#2677,#2679,#1693,.T.);
#3336=EDGE_CURVE('',#2679,#2679,#2465,.T.);
#3337=EDGE_CURVE('',#2680,#2681,#1694,.T.);
#3338=EDGE_CURVE('',#2682,#2680,#1695,.T.);
#3339=EDGE_CURVE('',#2683,#2682,#1696,.T.);
#3340=EDGE_CURVE('',#2683,#2681,#1697,.T.);
#3341=EDGE_CURVE('',#2684,#2685,#1698,.T.);
#3342=EDGE_CURVE('',#2684,#2686,#1699,.T.);
#3343=EDGE_CURVE('',#2687,#2686,#1700,.T.);
#3344=EDGE_CURVE('',#2685,#2687,#1701,.T.);
#3345=EDGE_CURVE('',#2688,#2689,#1702,.T.);
#3346=EDGE_CURVE('',#2688,#2690,#1703,.T.);
#3347=EDGE_CURVE('',#2691,#2690,#1704,.T.);
#3348=EDGE_CURVE('',#2689,#2691,#1705,.T.);
#3349=EDGE_CURVE('',#2692,#2693,#1706,.T.);
#3350=EDGE_CURVE('',#2692,#2694,#1707,.T.);
#3351=EDGE_CURVE('',#2695,#2694,#1708,.T.);
#3352=EDGE_CURVE('',#2693,#2695,#1709,.T.);
#3353=EDGE_CURVE('',#2696,#2697,#1710,.T.);
#3354=EDGE_CURVE('',#2696,#2698,#1711,.T.);
#3355=EDGE_CURVE('',#2699,#2698,#1712,.T.);
#3356=EDGE_CURVE('',#2697,#2699,#1713,.T.);
#3357=EDGE_CURVE('',#2700,#2701,#1714,.T.);
#3358=EDGE_CURVE('',#2702,#2700,#1715,.T.);
#3359=EDGE_CURVE('',#2703,#2702,#1716,.T.);
#3360=EDGE_CURVE('',#2703,#2701,#1717,.T.);
#3361=EDGE_CURVE('',#2704,#2705,#1718,.T.);
#3362=EDGE_CURVE('',#2706,#2704,#1719,.T.);
#3363=EDGE_CURVE('',#2707,#2706,#1720,.T.);
#3364=EDGE_CURVE('',#2707,#2705,#1721,.T.);
#3365=EDGE_CURVE('',#2708,#2708,#2466,.T.);
#3366=EDGE_CURVE('',#2709,#2709,#2467,.T.);
#3367=EDGE_CURVE('',#2681,#2696,#1722,.T.);
#3368=EDGE_CURVE('',#2698,#2683,#1723,.T.);
#3369=EDGE_CURVE('',#2701,#2684,#1724,.T.);
#3370=EDGE_CURVE('',#2686,#2703,#1725,.T.);
#3371=EDGE_CURVE('',#2705,#2688,#1726,.T.);
#3372=EDGE_CURVE('',#2690,#2707,#1727,.T.);
#3373=EDGE_CURVE('',#2710,#2692,#1728,.T.);
#3374=EDGE_CURVE('',#2711,#2710,#1729,.T.);
#3375=EDGE_CURVE('',#2694,#2711,#1730,.T.);
#3376=EDGE_CURVE('',#2712,#2710,#1731,.T.);
#3377=EDGE_CURVE('',#2713,#2712,#1732,.T.);
#3378=EDGE_CURVE('',#2711,#2713,#1733,.T.);
#3379=EDGE_CURVE('',#2714,#2715,#1734,.T.);
#3380=EDGE_CURVE('',#2716,#2715,#188,.T.);
#3381=EDGE_CURVE('',#2662,#2716,#189,.T.);
#3382=EDGE_CURVE('',#2714,#2659,#190,.T.);
#3383=EDGE_CURVE('',#2713,#2717,#1735,.T.);
#3384=EDGE_CURVE('',#2658,#2717,#191,.T.);
#3385=EDGE_CURVE('',#2718,#2661,#192,.T.);
#3386=EDGE_CURVE('',#2719,#2718,#193,.T.);
#3387=EDGE_CURVE('',#2719,#2695,#1736,.T.);
#3388=EDGE_CURVE('',#2706,#2720,#1737,.T.);
#3389=EDGE_CURVE('',#2721,#2720,#194,.T.);
#3390=EDGE_CURVE('',#2722,#2721,#195,.T.);
#3391=EDGE_CURVE('',#2723,#2722,#1738,.T.);
#3392=EDGE_CURVE('',#2724,#2723,#196,.T.);
#3393=EDGE_CURVE('',#2725,#2724,#197,.T.);
#3394=EDGE_CURVE('',#2725,#2691,#1739,.T.);
#3395=EDGE_CURVE('',#2702,#2726,#1740,.T.);
#3396=EDGE_CURVE('',#2654,#2726,#198,.T.);
#3397=EDGE_CURVE('',#2727,#2653,#1741,.T.);
#3398=EDGE_CURVE('',#2728,#2727,#199,.T.);
#3399=EDGE_CURVE('',#2729,#2728,#200,.T.);
#3400=EDGE_CURVE('',#2729,#2687,#1742,.T.);
#3401=EDGE_CURVE('',#2730,#2697,#1743,.T.);
#3402=EDGE_CURVE('',#2730,#2731,#201,.T.);
#3403=EDGE_CURVE('',#2731,#2732,#1744,.T.);
#3404=EDGE_CURVE('',#2732,#2733,#202,.T.);
#3405=EDGE_CURVE('',#2680,#2733,#1745,.T.);
#3406=EDGE_CURVE('',#2719,#2715,#203,.T.);
#3407=EDGE_CURVE('',#2714,#2717,#204,.T.);
#3408=EDGE_CURVE('',#2734,#2712,#1746,.T.);
#3409=EDGE_CURVE('',#2734,#2720,#205,.T.);
#3410=EDGE_CURVE('',#2735,#2704,#1747,.T.);
#3411=EDGE_CURVE('',#2735,#2726,#206,.T.);
#3412=EDGE_CURVE('',#2736,#2700,#1748,.T.);
#3413=EDGE_CURVE('',#2736,#2737,#207,.T.);
#3414=EDGE_CURVE('',#2737,#2730,#208,.T.);
#3415=EDGE_CURVE('',#2699,#2738,#1749,.T.);
#3416=EDGE_CURVE('',#2739,#2738,#209,.T.);
#3417=EDGE_CURVE('',#2739,#2740,#210,.T.);
#3418=EDGE_CURVE('',#2741,#2740,#211,.T.);
#3419=EDGE_CURVE('',#2741,#2742,#1750,.T.);
#3420=EDGE_CURVE('',#2743,#2742,#212,.T.);
#3421=EDGE_CURVE('',#2743,#2744,#213,.T.);
#3422=EDGE_CURVE('',#2745,#2744,#214,.T.);
#3423=EDGE_CURVE('',#2745,#2682,#1751,.T.);
#3424=EDGE_CURVE('',#2733,#2746,#215,.T.);
#3425=EDGE_CURVE('',#2746,#2747,#216,.T.);
#3426=EDGE_CURVE('',#2685,#2747,#1752,.T.);
#3427=EDGE_CURVE('',#2729,#2748,#217,.T.);
#3428=EDGE_CURVE('',#2689,#2748,#1753,.T.);
#3429=EDGE_CURVE('',#2725,#2749,#218,.T.);
#3430=EDGE_CURVE('',#2693,#2749,#1754,.T.);
#3431=EDGE_CURVE('',#2750,#2751,#219,.T.);
#3432=EDGE_CURVE('',#2751,#2752,#220,.T.);
#3433=EDGE_CURVE('',#2752,#2753,#1755,.T.);
#3434=EDGE_CURVE('',#2753,#2754,#221,.T.);
#3435=EDGE_CURVE('',#2754,#2755,#222,.T.);
#3436=EDGE_CURVE('',#2750,#2755,#1756,.T.);
#3437=EDGE_CURVE('',#2665,#2709,#1757,.T.);
#3438=EDGE_CURVE('',#2756,#2756,#2468,.T.);
#3439=EDGE_CURVE('',#2756,#2708,#1758,.T.);
#3440=EDGE_CURVE('',#2750,#2757,#223,.T.);
#3441=EDGE_CURVE('',#2758,#2755,#224,.T.);
#3442=EDGE_CURVE('',#2759,#2758,#225,.T.);
#3443=EDGE_CURVE('',#2760,#2759,#1759,.T.);
#3444=EDGE_CURVE('',#2757,#2760,#226,.T.);
#3445=EDGE_CURVE('',#2718,#2716,#227,.T.);
#3446=EDGE_CURVE('',#2757,#2761,#228,.T.);
#3447=EDGE_CURVE('',#2761,#2751,#229,.T.);
#3448=EDGE_CURVE('',#2762,#2760,#230,.T.);
#3449=EDGE_CURVE('',#2761,#2762,#2469,.F.);
#3450=EDGE_CURVE('',#2759,#2763,#231,.T.);
#3451=EDGE_CURVE('',#2763,#2762,#1760,.T.);
#3452=EDGE_CURVE('',#2754,#2764,#232,.T.);
#3453=EDGE_CURVE('',#2764,#2758,#233,.T.);
#3454=EDGE_CURVE('',#2765,#2749,#234,.T.);
#3455=EDGE_CURVE('',#2766,#2765,#235,.T.);
#3456=EDGE_CURVE('',#2767,#2766,#1761,.T.);
#3457=EDGE_CURVE('',#2768,#2767,#236,.T.);
#3458=EDGE_CURVE('',#2734,#2768,#237,.T.);
#3459=EDGE_CURVE('',#2724,#2765,#238,.T.);
#3460=EDGE_CURVE('',#2766,#2723,#239,.T.);
#3461=EDGE_CURVE('',#2722,#2767,#240,.T.);
#3462=EDGE_CURVE('',#2768,#2721,#241,.T.);
#3463=EDGE_CURVE('',#2769,#2748,#242,.T.);
#3464=EDGE_CURVE('',#2770,#2769,#243,.T.);
#3465=EDGE_CURVE('',#2656,#2770,#1762,.T.);
#3466=EDGE_CURVE('',#2735,#2655,#244,.T.);
#3467=EDGE_CURVE('',#2728,#2769,#245,.T.);
#3468=EDGE_CURVE('',#2770,#2650,#246,.T.);
#3469=EDGE_CURVE('',#2649,#2727,#247,.T.);
#3470=EDGE_CURVE('',#2771,#2747,#248,.T.);
#3471=EDGE_CURVE('',#2772,#2771,#249,.T.);
#3472=EDGE_CURVE('',#2773,#2772,#1763,.T.);
#3473=EDGE_CURVE('',#2774,#2773,#250,.T.);
#3474=EDGE_CURVE('',#2736,#2774,#251,.T.);
#3475=EDGE_CURVE('',#2746,#2775,#252,.T.);
#3476=EDGE_CURVE('',#2775,#2771,#253,.T.);
#3477=EDGE_CURVE('',#2776,#2775,#2470,.F.);
#3478=EDGE_CURVE('',#2772,#2776,#254,.T.);
#3479=EDGE_CURVE('',#2776,#2777,#1764,.T.);
#3480=EDGE_CURVE('',#2777,#2773,#255,.T.);
#3481=EDGE_CURVE('',#2774,#2778,#256,.T.);
#3482=EDGE_CURVE('',#2778,#2737,#257,.T.);
#3483=EDGE_CURVE('',#2778,#2777,#2471,.F.);
#3484=EDGE_CURVE('',#2777,#2731,#2472,.F.);
#3485=EDGE_CURVE('',#2731,#2778,#2473,.F.);
#3486=EDGE_CURVE('',#2763,#2764,#2474,.F.);
#3487=EDGE_CURVE('',#2764,#2779,#2475,.F.);
#3488=EDGE_CURVE('',#2779,#2763,#2476,.F.);
#3489=EDGE_CURVE('',#2775,#2732,#2477,.F.);
#3490=EDGE_CURVE('',#2732,#2776,#2478,.F.);
#3491=EDGE_CURVE('',#2780,#2761,#2479,.F.);
#3492=EDGE_CURVE('',#2762,#2780,#2480,.F.);
#3493=EDGE_CURVE('',#2780,#2779,#1765,.T.);
#3494=EDGE_CURVE('',#2752,#2780,#258,.T.);
#3495=EDGE_CURVE('',#2779,#2753,#259,.T.);
#3496=EDGE_CURVE('',#2781,#2782,#2481,.F.);
#3497=EDGE_CURVE('',#2783,#2781,#2482,.F.);
#3498=EDGE_CURVE('',#2782,#2783,#2483,.F.);
#3499=EDGE_CURVE('',#2784,#2785,#2484,.F.);
#3500=EDGE_CURVE('',#2786,#2784,#2485,.F.);
#3501=EDGE_CURVE('',#2785,#2786,#2486,.F.);
#3502=EDGE_CURVE('',#2787,#2788,#2487,.F.);
#3503=EDGE_CURVE('',#2789,#2787,#2488,.F.);
#3504=EDGE_CURVE('',#2788,#2789,#2489,.F.);
#3505=EDGE_CURVE('',#2782,#2789,#1766,.T.);
#3506=EDGE_CURVE('',#2787,#2781,#1767,.T.);
#3507=EDGE_CURVE('',#2744,#2788,#260,.T.);
#3508=EDGE_CURVE('',#2789,#2745,#261,.T.);
#3509=EDGE_CURVE('',#2790,#2791,#2490,.F.);
#3510=EDGE_CURVE('',#2792,#2790,#2491,.F.);
#3511=EDGE_CURVE('',#2791,#2792,#2492,.F.);
#3512=EDGE_CURVE('',#2790,#2786,#1768,.T.);
#3513=EDGE_CURVE('',#2784,#2792,#1769,.T.);
#3514=EDGE_CURVE('',#2788,#2791,#262,.T.);
#3515=EDGE_CURVE('',#2792,#2787,#263,.T.);
#3516=EDGE_CURVE('',#2742,#2790,#264,.T.);
#3517=EDGE_CURVE('',#2791,#2743,#265,.T.);
#3518=EDGE_CURVE('',#2740,#2785,#266,.T.);
#3519=EDGE_CURVE('',#2786,#2741,#267,.T.);
#3520=EDGE_CURVE('',#2785,#2783,#268,.T.);
#3521=EDGE_CURVE('',#2781,#2784,#269,.T.);
#3522=EDGE_CURVE('',#2738,#2782,#270,.T.);
#3523=EDGE_CURVE('',#2783,#2739,#271,.T.);
#3524=EDGE_CURVE('',#2793,#2794,#272,.T.);
#3525=EDGE_CURVE('',#2793,#2794,#2493,.T.);
#3526=EDGE_CURVE('',#2795,#2796,#273,.T.);
#3527=EDGE_CURVE('',#2795,#2796,#2494,.T.);
#3528=EDGE_CURVE('',#2797,#2798,#274,.T.);
#3529=EDGE_CURVE('',#2797,#2798,#2495,.T.);
#3530=EDGE_CURVE('',#2799,#2800,#275,.T.);
#3531=EDGE_CURVE('',#2799,#2800,#2496,.T.);
#3532=EDGE_CURVE('',#2801,#2796,#276,.T.);
#3533=EDGE_CURVE('',#2801,#2802,#277,.T.);
#3534=EDGE_CURVE('',#2803,#2802,#278,.T.);
#3535=EDGE_CURVE('',#2803,#2804,#279,.T.);
#3536=EDGE_CURVE('',#2795,#2804,#280,.T.);
#3537=EDGE_CURVE('',#2805,#2800,#281,.T.);
#3538=EDGE_CURVE('',#2805,#2806,#282,.T.);
#3539=EDGE_CURVE('',#2807,#2806,#283,.T.);
#3540=EDGE_CURVE('',#2807,#2808,#284,.T.);
#3541=EDGE_CURVE('',#2799,#2808,#285,.T.);
#3542=EDGE_CURVE('',#2793,#2809,#286,.T.);
#3543=EDGE_CURVE('',#2809,#2805,#1770,.T.);
#3544=EDGE_CURVE('',#2808,#2810,#1771,.T.);
#3545=EDGE_CURVE('',#2810,#2794,#287,.T.);
#3546=EDGE_CURVE('',#2811,#2811,#2497,.T.);
#3547=EDGE_CURVE('',#2812,#2812,#2498,.T.);
#3548=EDGE_CURVE('',#2813,#2813,#2499,.T.);
#3549=EDGE_CURVE('',#2814,#2815,#1772,.T.);
#3550=EDGE_CURVE('',#2814,#2816,#1773,.T.);
#3551=EDGE_CURVE('',#2816,#2817,#1774,.T.);
#3552=EDGE_CURVE('',#2815,#2817,#1775,.T.);
#3553=EDGE_CURVE('',#2818,#2814,#1776,.T.);
#3554=EDGE_CURVE('',#2818,#2819,#1777,.T.);
#3555=EDGE_CURVE('',#2819,#2816,#1778,.T.);
#3556=EDGE_CURVE('',#2820,#2818,#1779,.T.);
#3557=EDGE_CURVE('',#2820,#2821,#1780,.T.);
#3558=EDGE_CURVE('',#2821,#2819,#1781,.T.);
#3559=EDGE_CURVE('',#2822,#2820,#1782,.T.);
#3560=EDGE_CURVE('',#2822,#2823,#1783,.T.);
#3561=EDGE_CURVE('',#2823,#2821,#1784,.T.);
#3562=EDGE_CURVE('',#2824,#2822,#1785,.T.);
#3563=EDGE_CURVE('',#2824,#2825,#1786,.T.);
#3564=EDGE_CURVE('',#2825,#2823,#1787,.T.);
#3565=EDGE_CURVE('',#2815,#2824,#1788,.T.);
#3566=EDGE_CURVE('',#2817,#2825,#1789,.T.);
#3567=EDGE_CURVE('',#2826,#2826,#2500,.T.);
#3568=EDGE_CURVE('',#2827,#2828,#1790,.T.);
#3569=EDGE_CURVE('',#2827,#2829,#1791,.T.);
#3570=EDGE_CURVE('',#2829,#2830,#1792,.T.);
#3571=EDGE_CURVE('',#2828,#2830,#1793,.T.);
#3572=EDGE_CURVE('',#2831,#2827,#1794,.T.);
#3573=EDGE_CURVE('',#2831,#2832,#1795,.T.);
#3574=EDGE_CURVE('',#2832,#2829,#1796,.T.);
#3575=EDGE_CURVE('',#2833,#2831,#1797,.T.);
#3576=EDGE_CURVE('',#2833,#2834,#1798,.T.);
#3577=EDGE_CURVE('',#2834,#2832,#1799,.T.);
#3578=EDGE_CURVE('',#2835,#2833,#1800,.T.);
#3579=EDGE_CURVE('',#2835,#2836,#1801,.T.);
#3580=EDGE_CURVE('',#2836,#2834,#1802,.T.);
#3581=EDGE_CURVE('',#2837,#2835,#1803,.T.);
#3582=EDGE_CURVE('',#2837,#2838,#1804,.T.);
#3583=EDGE_CURVE('',#2838,#2836,#1805,.T.);
#3584=EDGE_CURVE('',#2828,#2837,#1806,.T.);
#3585=EDGE_CURVE('',#2830,#2838,#1807,.T.);
#3586=EDGE_CURVE('',#2839,#2839,#2501,.T.);
#3587=EDGE_CURVE('',#2840,#2840,#2502,.T.);
#3588=EDGE_CURVE('',#2840,#2811,#1808,.T.);
#3589=EDGE_CURVE('',#2841,#2841,#2503,.T.);
#3590=EDGE_CURVE('',#2841,#2842,#1809,.T.);
#3591=EDGE_CURVE('',#2842,#2842,#2504,.T.);
#3592=EDGE_CURVE('',#2843,#2843,#2505,.T.);
#3593=EDGE_CURVE('',#2843,#2844,#1810,.T.);
#3594=EDGE_CURVE('',#2844,#2844,#2506,.T.);
#3595=EDGE_CURVE('',#2845,#2845,#2507,.T.);
#3596=EDGE_CURVE('',#2845,#2812,#1811,.T.);
#3597=EDGE_CURVE('',#2839,#2846,#1812,.T.);
#3598=EDGE_CURVE('',#2846,#2846,#2508,.T.);
#3599=EDGE_CURVE('',#2826,#2847,#1813,.T.);
#3600=EDGE_CURVE('',#2847,#2847,#2509,.T.);
#3601=EDGE_CURVE('',#2848,#2849,#1814,.T.);
#3602=EDGE_CURVE('',#2850,#2848,#1815,.T.);
#3603=EDGE_CURVE('',#2851,#2850,#1816,.T.);
#3604=EDGE_CURVE('',#2851,#2849,#1817,.T.);
#3605=EDGE_CURVE('',#2852,#2853,#1818,.T.);
#3606=EDGE_CURVE('',#2852,#2854,#1819,.T.);
#3607=EDGE_CURVE('',#2855,#2854,#1820,.T.);
#3608=EDGE_CURVE('',#2853,#2855,#1821,.T.);
#3609=EDGE_CURVE('',#2856,#2857,#1822,.T.);
#3610=EDGE_CURVE('',#2856,#2858,#1823,.T.);
#3611=EDGE_CURVE('',#2859,#2858,#1824,.T.);
#3612=EDGE_CURVE('',#2857,#2859,#1825,.T.);
#3613=EDGE_CURVE('',#2860,#2861,#1826,.T.);
#3614=EDGE_CURVE('',#2860,#2862,#1827,.T.);
#3615=EDGE_CURVE('',#2863,#2862,#1828,.T.);
#3616=EDGE_CURVE('',#2861,#2863,#1829,.T.);
#3617=EDGE_CURVE('',#2864,#2865,#1830,.T.);
#3618=EDGE_CURVE('',#2864,#2866,#1831,.T.);
#3619=EDGE_CURVE('',#2867,#2866,#1832,.T.);
#3620=EDGE_CURVE('',#2865,#2867,#1833,.T.);
#3621=EDGE_CURVE('',#2868,#2869,#1834,.T.);
#3622=EDGE_CURVE('',#2870,#2868,#1835,.T.);
#3623=EDGE_CURVE('',#2871,#2870,#1836,.T.);
#3624=EDGE_CURVE('',#2871,#2869,#1837,.T.);
#3625=EDGE_CURVE('',#2872,#2873,#1838,.T.);
#3626=EDGE_CURVE('',#2874,#2872,#1839,.T.);
#3627=EDGE_CURVE('',#2875,#2874,#1840,.T.);
#3628=EDGE_CURVE('',#2875,#2873,#1841,.T.);
#3629=EDGE_CURVE('',#2876,#2876,#2510,.T.);
#3630=EDGE_CURVE('',#2877,#2877,#2511,.T.);
#3631=EDGE_CURVE('',#2849,#2864,#1842,.T.);
#3632=EDGE_CURVE('',#2866,#2851,#1843,.T.);
#3633=EDGE_CURVE('',#2869,#2852,#1844,.T.);
#3634=EDGE_CURVE('',#2854,#2871,#1845,.T.);
#3635=EDGE_CURVE('',#2873,#2856,#1846,.T.);
#3636=EDGE_CURVE('',#2858,#2875,#1847,.T.);
#3637=EDGE_CURVE('',#2878,#2860,#1848,.T.);
#3638=EDGE_CURVE('',#2879,#2878,#1849,.T.);
#3639=EDGE_CURVE('',#2862,#2879,#1850,.T.);
#3640=EDGE_CURVE('',#2880,#2878,#1851,.T.);
#3641=EDGE_CURVE('',#2881,#2880,#1852,.T.);
#3642=EDGE_CURVE('',#2879,#2881,#1853,.T.);
#3643=EDGE_CURVE('',#2882,#2883,#1854,.T.);
#3644=EDGE_CURVE('',#2884,#2883,#288,.T.);
#3645=EDGE_CURVE('',#2810,#2884,#289,.T.);
#3646=EDGE_CURVE('',#2882,#2807,#290,.T.);
#3647=EDGE_CURVE('',#2881,#2885,#1855,.T.);
#3648=EDGE_CURVE('',#2806,#2885,#291,.T.);
#3649=EDGE_CURVE('',#2886,#2809,#292,.T.);
#3650=EDGE_CURVE('',#2887,#2886,#293,.T.);
#3651=EDGE_CURVE('',#2887,#2863,#1856,.T.);
#3652=EDGE_CURVE('',#2874,#2888,#1857,.T.);
#3653=EDGE_CURVE('',#2889,#2888,#294,.T.);
#3654=EDGE_CURVE('',#2890,#2889,#295,.T.);
#3655=EDGE_CURVE('',#2891,#2890,#1858,.T.);
#3656=EDGE_CURVE('',#2892,#2891,#296,.T.);
#3657=EDGE_CURVE('',#2893,#2892,#297,.T.);
#3658=EDGE_CURVE('',#2893,#2859,#1859,.T.);
#3659=EDGE_CURVE('',#2870,#2894,#1860,.T.);
#3660=EDGE_CURVE('',#2802,#2894,#298,.T.);
#3661=EDGE_CURVE('',#2895,#2801,#1861,.T.);
#3662=EDGE_CURVE('',#2896,#2895,#299,.T.);
#3663=EDGE_CURVE('',#2897,#2896,#300,.T.);
#3664=EDGE_CURVE('',#2897,#2855,#1862,.T.);
#3665=EDGE_CURVE('',#2898,#2865,#1863,.T.);
#3666=EDGE_CURVE('',#2898,#2899,#301,.T.);
#3667=EDGE_CURVE('',#2899,#2900,#1864,.T.);
#3668=EDGE_CURVE('',#2900,#2901,#302,.T.);
#3669=EDGE_CURVE('',#2848,#2901,#1865,.T.);
#3670=EDGE_CURVE('',#2887,#2883,#303,.T.);
#3671=EDGE_CURVE('',#2882,#2885,#304,.T.);
#3672=EDGE_CURVE('',#2902,#2880,#1866,.T.);
#3673=EDGE_CURVE('',#2902,#2888,#305,.T.);
#3674=EDGE_CURVE('',#2903,#2872,#1867,.T.);
#3675=EDGE_CURVE('',#2903,#2894,#306,.T.);
#3676=EDGE_CURVE('',#2904,#2868,#1868,.T.);
#3677=EDGE_CURVE('',#2904,#2905,#307,.T.);
#3678=EDGE_CURVE('',#2905,#2898,#308,.T.);
#3679=EDGE_CURVE('',#2867,#2906,#1869,.T.);
#3680=EDGE_CURVE('',#2907,#2906,#309,.T.);
#3681=EDGE_CURVE('',#2907,#2908,#310,.T.);
#3682=EDGE_CURVE('',#2909,#2908,#311,.T.);
#3683=EDGE_CURVE('',#2909,#2910,#1870,.T.);
#3684=EDGE_CURVE('',#2911,#2910,#312,.T.);
#3685=EDGE_CURVE('',#2911,#2912,#313,.T.);
#3686=EDGE_CURVE('',#2913,#2912,#314,.T.);
#3687=EDGE_CURVE('',#2913,#2850,#1871,.T.);
#3688=EDGE_CURVE('',#2901,#2914,#315,.T.);
#3689=EDGE_CURVE('',#2914,#2915,#316,.T.);
#3690=EDGE_CURVE('',#2853,#2915,#1872,.T.);
#3691=EDGE_CURVE('',#2897,#2916,#317,.T.);
#3692=EDGE_CURVE('',#2857,#2916,#1873,.T.);
#3693=EDGE_CURVE('',#2893,#2917,#318,.T.);
#3694=EDGE_CURVE('',#2861,#2917,#1874,.T.);
#3695=EDGE_CURVE('',#2918,#2919,#319,.T.);
#3696=EDGE_CURVE('',#2919,#2920,#320,.T.);
#3697=EDGE_CURVE('',#2920,#2921,#1875,.T.);
#3698=EDGE_CURVE('',#2921,#2922,#321,.T.);
#3699=EDGE_CURVE('',#2922,#2923,#322,.T.);
#3700=EDGE_CURVE('',#2918,#2923,#1876,.T.);
#3701=EDGE_CURVE('',#2813,#2877,#1877,.T.);
#3702=EDGE_CURVE('',#2924,#2924,#2512,.T.);
#3703=EDGE_CURVE('',#2924,#2876,#1878,.T.);
#3704=EDGE_CURVE('',#2918,#2925,#323,.T.);
#3705=EDGE_CURVE('',#2926,#2923,#324,.T.);
#3706=EDGE_CURVE('',#2927,#2926,#325,.T.);
#3707=EDGE_CURVE('',#2928,#2927,#1879,.T.);
#3708=EDGE_CURVE('',#2925,#2928,#326,.T.);
#3709=EDGE_CURVE('',#2886,#2884,#327,.T.);
#3710=EDGE_CURVE('',#2925,#2929,#328,.T.);
#3711=EDGE_CURVE('',#2929,#2919,#329,.T.);
#3712=EDGE_CURVE('',#2930,#2928,#330,.T.);
#3713=EDGE_CURVE('',#2929,#2930,#2513,.F.);
#3714=EDGE_CURVE('',#2927,#2931,#331,.T.);
#3715=EDGE_CURVE('',#2931,#2930,#1880,.T.);
#3716=EDGE_CURVE('',#2922,#2932,#332,.T.);
#3717=EDGE_CURVE('',#2932,#2926,#333,.T.);
#3718=EDGE_CURVE('',#2933,#2917,#334,.T.);
#3719=EDGE_CURVE('',#2934,#2933,#335,.T.);
#3720=EDGE_CURVE('',#2935,#2934,#1881,.T.);
#3721=EDGE_CURVE('',#2936,#2935,#336,.T.);
#3722=EDGE_CURVE('',#2902,#2936,#337,.T.);
#3723=EDGE_CURVE('',#2892,#2933,#338,.T.);
#3724=EDGE_CURVE('',#2934,#2891,#339,.T.);
#3725=EDGE_CURVE('',#2890,#2935,#340,.T.);
#3726=EDGE_CURVE('',#2936,#2889,#341,.T.);
#3727=EDGE_CURVE('',#2937,#2916,#342,.T.);
#3728=EDGE_CURVE('',#2938,#2937,#343,.T.);
#3729=EDGE_CURVE('',#2804,#2938,#1882,.T.);
#3730=EDGE_CURVE('',#2903,#2803,#344,.T.);
#3731=EDGE_CURVE('',#2896,#2937,#345,.T.);
#3732=EDGE_CURVE('',#2938,#2798,#346,.T.);
#3733=EDGE_CURVE('',#2797,#2895,#347,.T.);
#3734=EDGE_CURVE('',#2939,#2915,#348,.T.);
#3735=EDGE_CURVE('',#2940,#2939,#349,.T.);
#3736=EDGE_CURVE('',#2941,#2940,#1883,.T.);
#3737=EDGE_CURVE('',#2942,#2941,#350,.T.);
#3738=EDGE_CURVE('',#2904,#2942,#351,.T.);
#3739=EDGE_CURVE('',#2914,#2943,#352,.T.);
#3740=EDGE_CURVE('',#2943,#2939,#353,.T.);
#3741=EDGE_CURVE('',#2944,#2943,#2514,.F.);
#3742=EDGE_CURVE('',#2940,#2944,#354,.T.);
#3743=EDGE_CURVE('',#2944,#2945,#1884,.T.);
#3744=EDGE_CURVE('',#2945,#2941,#355,.T.);
#3745=EDGE_CURVE('',#2942,#2946,#356,.T.);
#3746=EDGE_CURVE('',#2946,#2905,#357,.T.);
#3747=EDGE_CURVE('',#2946,#2945,#2515,.F.);
#3748=EDGE_CURVE('',#2945,#2899,#2516,.F.);
#3749=EDGE_CURVE('',#2899,#2946,#2517,.F.);
#3750=EDGE_CURVE('',#2931,#2932,#2518,.F.);
#3751=EDGE_CURVE('',#2932,#2947,#2519,.F.);
#3752=EDGE_CURVE('',#2947,#2931,#2520,.F.);
#3753=EDGE_CURVE('',#2943,#2900,#2521,.F.);
#3754=EDGE_CURVE('',#2900,#2944,#2522,.F.);
#3755=EDGE_CURVE('',#2948,#2929,#2523,.F.);
#3756=EDGE_CURVE('',#2930,#2948,#2524,.F.);
#3757=EDGE_CURVE('',#2948,#2947,#1885,.T.);
#3758=EDGE_CURVE('',#2920,#2948,#358,.T.);
#3759=EDGE_CURVE('',#2947,#2921,#359,.T.);
#3760=EDGE_CURVE('',#2949,#2950,#2525,.F.);
#3761=EDGE_CURVE('',#2951,#2949,#2526,.F.);
#3762=EDGE_CURVE('',#2950,#2951,#2527,.F.);
#3763=EDGE_CURVE('',#2952,#2953,#2528,.F.);
#3764=EDGE_CURVE('',#2954,#2952,#2529,.F.);
#3765=EDGE_CURVE('',#2953,#2954,#2530,.F.);
#3766=EDGE_CURVE('',#2955,#2956,#2531,.F.);
#3767=EDGE_CURVE('',#2957,#2955,#2532,.F.);
#3768=EDGE_CURVE('',#2956,#2957,#2533,.F.);
#3769=EDGE_CURVE('',#2950,#2957,#1886,.T.);
#3770=EDGE_CURVE('',#2955,#2949,#1887,.T.);
#3771=EDGE_CURVE('',#2912,#2956,#360,.T.);
#3772=EDGE_CURVE('',#2957,#2913,#361,.T.);
#3773=EDGE_CURVE('',#2958,#2959,#2534,.F.);
#3774=EDGE_CURVE('',#2960,#2958,#2535,.F.);
#3775=EDGE_CURVE('',#2959,#2960,#2536,.F.);
#3776=EDGE_CURVE('',#2958,#2954,#1888,.T.);
#3777=EDGE_CURVE('',#2952,#2960,#1889,.T.);
#3778=EDGE_CURVE('',#2956,#2959,#362,.T.);
#3779=EDGE_CURVE('',#2960,#2955,#363,.T.);
#3780=EDGE_CURVE('',#2910,#2958,#364,.T.);
#3781=EDGE_CURVE('',#2959,#2911,#365,.T.);
#3782=EDGE_CURVE('',#2908,#2953,#366,.T.);
#3783=EDGE_CURVE('',#2954,#2909,#367,.T.);
#3784=EDGE_CURVE('',#2953,#2951,#368,.T.);
#3785=EDGE_CURVE('',#2949,#2952,#369,.T.);
#3786=EDGE_CURVE('',#2906,#2950,#370,.T.);
#3787=EDGE_CURVE('',#2951,#2907,#371,.T.);
#3788=EDGE_CURVE('',#2961,#2962,#1890,.T.);
#3789=EDGE_CURVE('',#2961,#2963,#372,.T.);
#3790=EDGE_CURVE('',#2963,#2964,#2537,.F.);
#3791=EDGE_CURVE('',#2964,#2962,#373,.T.);
#3792=EDGE_CURVE('',#2965,#2966,#1891,.T.);
#3793=EDGE_CURVE('',#2965,#2961,#374,.T.);
#3794=EDGE_CURVE('',#2962,#2966,#375,.T.);
#3795=EDGE_CURVE('',#2967,#2968,#1892,.T.);
#3796=EDGE_CURVE('',#2967,#2965,#376,.T.);
#3797=EDGE_CURVE('',#2966,#2968,#377,.T.);
#3798=EDGE_CURVE('',#2969,#2970,#1893,.T.);
#3799=EDGE_CURVE('',#2969,#2967,#378,.T.);
#3800=EDGE_CURVE('',#2968,#2970,#379,.T.);
#3801=EDGE_CURVE('',#2971,#2972,#1894,.T.);
#3802=EDGE_CURVE('',#2971,#2969,#380,.T.);
#3803=EDGE_CURVE('',#2970,#2972,#381,.T.);
#3804=EDGE_CURVE('',#2973,#2974,#1895,.T.);
#3805=EDGE_CURVE('',#2973,#2971,#382,.T.);
#3806=EDGE_CURVE('',#2972,#2974,#383,.T.);
#3807=EDGE_CURVE('',#2975,#2976,#1896,.T.);
#3808=EDGE_CURVE('',#2975,#2973,#384,.T.);
#3809=EDGE_CURVE('',#2974,#2976,#385,.T.);
#3810=EDGE_CURVE('',#2977,#2978,#1897,.T.);
#3811=EDGE_CURVE('',#2977,#2975,#386,.T.);
#3812=EDGE_CURVE('',#2976,#2978,#387,.T.);
#3813=EDGE_CURVE('',#2979,#2980,#1898,.T.);
#3814=EDGE_CURVE('',#2979,#2977,#388,.T.);
#3815=EDGE_CURVE('',#2978,#2980,#389,.T.);
#3816=EDGE_CURVE('',#2981,#2982,#1899,.T.);
#3817=EDGE_CURVE('',#2981,#2979,#390,.T.);
#3818=EDGE_CURVE('',#2980,#2982,#391,.T.);
#3819=EDGE_CURVE('',#2983,#2984,#1900,.T.);
#3820=EDGE_CURVE('',#2983,#2981,#392,.T.);
#3821=EDGE_CURVE('',#2982,#2984,#393,.T.);
#3822=EDGE_CURVE('',#2985,#2986,#1901,.T.);
#3823=EDGE_CURVE('',#2985,#2983,#394,.T.);
#3824=EDGE_CURVE('',#2984,#2986,#395,.T.);
#3825=EDGE_CURVE('',#2987,#2988,#1902,.T.);
#3826=EDGE_CURVE('',#2987,#2985,#396,.T.);
#3827=EDGE_CURVE('',#2986,#2988,#397,.T.);
#3828=EDGE_CURVE('',#2989,#2990,#1903,.T.);
#3829=EDGE_CURVE('',#2989,#2987,#398,.T.);
#3830=EDGE_CURVE('',#2988,#2990,#399,.T.);
#3831=EDGE_CURVE('',#2991,#2992,#1904,.T.);
#3832=EDGE_CURVE('',#2991,#2989,#400,.T.);
#3833=EDGE_CURVE('',#2990,#2992,#401,.T.);
#3834=EDGE_CURVE('',#2993,#2994,#1905,.T.);
#3835=EDGE_CURVE('',#2993,#2991,#402,.T.);
#3836=EDGE_CURVE('',#2992,#2994,#403,.T.);
#3837=EDGE_CURVE('',#2995,#2996,#1906,.T.);
#3838=EDGE_CURVE('',#2995,#2993,#404,.T.);
#3839=EDGE_CURVE('',#2994,#2996,#405,.T.);
#3840=EDGE_CURVE('',#2997,#2998,#1907,.T.);
#3841=EDGE_CURVE('',#2997,#2995,#406,.T.);
#3842=EDGE_CURVE('',#2996,#2998,#407,.T.);
#3843=EDGE_CURVE('',#2999,#3000,#1908,.T.);
#3844=EDGE_CURVE('',#2999,#2997,#408,.T.);
#3845=EDGE_CURVE('',#2998,#3000,#409,.T.);
#3846=EDGE_CURVE('',#3001,#3002,#1909,.T.);
#3847=EDGE_CURVE('',#3001,#2999,#410,.T.);
#3848=EDGE_CURVE('',#3000,#3002,#411,.T.);
#3849=EDGE_CURVE('',#3003,#3004,#1910,.T.);
#3850=EDGE_CURVE('',#3003,#3001,#412,.T.);
#3851=EDGE_CURVE('',#3002,#3004,#413,.T.);
#3852=EDGE_CURVE('',#3005,#3006,#1911,.T.);
#3853=EDGE_CURVE('',#3005,#3003,#414,.T.);
#3854=EDGE_CURVE('',#3004,#3006,#415,.T.);
#3855=EDGE_CURVE('',#3007,#3008,#1912,.T.);
#3856=EDGE_CURVE('',#3007,#3005,#416,.T.);
#3857=EDGE_CURVE('',#3006,#3008,#417,.T.);
#3858=EDGE_CURVE('',#3009,#3010,#1913,.T.);
#3859=EDGE_CURVE('',#3009,#3007,#418,.T.);
#3860=EDGE_CURVE('',#3008,#3010,#419,.T.);
#3861=EDGE_CURVE('',#3011,#3012,#1914,.T.);
#3862=EDGE_CURVE('',#3011,#3009,#420,.T.);
#3863=EDGE_CURVE('',#3010,#3012,#421,.T.);
#3864=EDGE_CURVE('',#3013,#3014,#1915,.T.);
#3865=EDGE_CURVE('',#3013,#3011,#422,.T.);
#3866=EDGE_CURVE('',#3012,#3014,#423,.T.);
#3867=EDGE_CURVE('',#3015,#3016,#1916,.T.);
#3868=EDGE_CURVE('',#3015,#3013,#424,.T.);
#3869=EDGE_CURVE('',#3014,#3016,#425,.T.);
#3870=EDGE_CURVE('',#3017,#3018,#1917,.T.);
#3871=EDGE_CURVE('',#3017,#3015,#426,.T.);
#3872=EDGE_CURVE('',#3016,#3018,#427,.T.);
#3873=EDGE_CURVE('',#3019,#3020,#1918,.T.);
#3874=EDGE_CURVE('',#3019,#3017,#428,.T.);
#3875=EDGE_CURVE('',#3018,#3020,#429,.T.);
#3876=EDGE_CURVE('',#3021,#3022,#1919,.T.);
#3877=EDGE_CURVE('',#3021,#3019,#430,.T.);
#3878=EDGE_CURVE('',#3020,#3022,#431,.T.);
#3879=EDGE_CURVE('',#3023,#3024,#1920,.T.);
#3880=EDGE_CURVE('',#3023,#3025,#432,.T.);
#3881=EDGE_CURVE('',#3025,#3026,#2538,.T.);
#3882=EDGE_CURVE('',#3024,#3026,#433,.T.);
#3883=EDGE_CURVE('',#3027,#3028,#1921,.T.);
#3884=EDGE_CURVE('',#3027,#3023,#434,.T.);
#3885=EDGE_CURVE('',#3028,#3024,#435,.T.);
#3886=EDGE_CURVE('',#3029,#3030,#1922,.T.);
#3887=EDGE_CURVE('',#3029,#3027,#436,.T.);
#3888=EDGE_CURVE('',#3030,#3028,#437,.T.);
#3889=EDGE_CURVE('',#3031,#3032,#1923,.T.);
#3890=EDGE_CURVE('',#3031,#3029,#438,.T.);
#3891=EDGE_CURVE('',#3032,#3030,#439,.T.);
#3892=EDGE_CURVE('',#3033,#3034,#1924,.T.);
#3893=EDGE_CURVE('',#3033,#3031,#440,.T.);
#3894=EDGE_CURVE('',#3034,#3032,#441,.T.);
#3895=EDGE_CURVE('',#3035,#3036,#1925,.T.);
#3896=EDGE_CURVE('',#3035,#3033,#442,.T.);
#3897=EDGE_CURVE('',#3036,#3034,#443,.T.);
#3898=EDGE_CURVE('',#3037,#3038,#1926,.T.);
#3899=EDGE_CURVE('',#3037,#3035,#444,.T.);
#3900=EDGE_CURVE('',#3038,#3036,#445,.T.);
#3901=EDGE_CURVE('',#3039,#3040,#1927,.T.);
#3902=EDGE_CURVE('',#3039,#3037,#446,.T.);
#3903=EDGE_CURVE('',#3040,#3038,#447,.T.);
#3904=EDGE_CURVE('',#3041,#3042,#1928,.T.);
#3905=EDGE_CURVE('',#3041,#3039,#448,.T.);
#3906=EDGE_CURVE('',#3042,#3040,#449,.T.);
#3907=EDGE_CURVE('',#3043,#3044,#1929,.T.);
#3908=EDGE_CURVE('',#3043,#3041,#450,.T.);
#3909=EDGE_CURVE('',#3044,#3042,#451,.T.);
#3910=EDGE_CURVE('',#3045,#3046,#1930,.T.);
#3911=EDGE_CURVE('',#3045,#3043,#452,.T.);
#3912=EDGE_CURVE('',#3046,#3044,#453,.T.);
#3913=EDGE_CURVE('',#3047,#3048,#1931,.T.);
#3914=EDGE_CURVE('',#3047,#3045,#454,.T.);
#3915=EDGE_CURVE('',#3048,#3046,#455,.T.);
#3916=EDGE_CURVE('',#3049,#3050,#1932,.T.);
#3917=EDGE_CURVE('',#3049,#3047,#456,.T.);
#3918=EDGE_CURVE('',#3050,#3048,#457,.T.);
#3919=EDGE_CURVE('',#3051,#3052,#1933,.T.);
#3920=EDGE_CURVE('',#3051,#3049,#458,.T.);
#3921=EDGE_CURVE('',#3052,#3050,#459,.T.);
#3922=EDGE_CURVE('',#3053,#3054,#1934,.T.);
#3923=EDGE_CURVE('',#3053,#3051,#460,.T.);
#3924=EDGE_CURVE('',#3054,#3052,#461,.T.);
#3925=EDGE_CURVE('',#3055,#3056,#1935,.T.);
#3926=EDGE_CURVE('',#3055,#3053,#462,.T.);
#3927=EDGE_CURVE('',#3056,#3054,#463,.T.);
#3928=EDGE_CURVE('',#3057,#3058,#1936,.T.);
#3929=EDGE_CURVE('',#3057,#3055,#464,.T.);
#3930=EDGE_CURVE('',#3058,#3056,#465,.T.);
#3931=EDGE_CURVE('',#3059,#3060,#1937,.T.);
#3932=EDGE_CURVE('',#3059,#3057,#466,.T.);
#3933=EDGE_CURVE('',#3060,#3058,#467,.T.);
#3934=EDGE_CURVE('',#3061,#3062,#1938,.T.);
#3935=EDGE_CURVE('',#3061,#3059,#468,.T.);
#3936=EDGE_CURVE('',#3062,#3060,#469,.T.);
#3937=EDGE_CURVE('',#3063,#3064,#1939,.T.);
#3938=EDGE_CURVE('',#3063,#3061,#470,.T.);
#3939=EDGE_CURVE('',#3064,#3062,#471,.T.);
#3940=EDGE_CURVE('',#3065,#3066,#1940,.T.);
#3941=EDGE_CURVE('',#3065,#3063,#472,.T.);
#3942=EDGE_CURVE('',#3066,#3064,#473,.T.);
#3943=EDGE_CURVE('',#3067,#3068,#1941,.T.);
#3944=EDGE_CURVE('',#3067,#3065,#474,.T.);
#3945=EDGE_CURVE('',#3068,#3066,#475,.T.);
#3946=EDGE_CURVE('',#3069,#3070,#1942,.T.);
#3947=EDGE_CURVE('',#3069,#3067,#476,.T.);
#3948=EDGE_CURVE('',#3070,#3068,#477,.T.);
#3949=EDGE_CURVE('',#3071,#3072,#1943,.T.);
#3950=EDGE_CURVE('',#3071,#3069,#478,.T.);
#3951=EDGE_CURVE('',#3072,#3070,#479,.T.);
#3952=EDGE_CURVE('',#3073,#3074,#1944,.T.);
#3953=EDGE_CURVE('',#3073,#3071,#480,.T.);
#3954=EDGE_CURVE('',#3074,#3072,#481,.T.);
#3955=EDGE_CURVE('',#3075,#3076,#1945,.T.);
#3956=EDGE_CURVE('',#3075,#3073,#482,.T.);
#3957=EDGE_CURVE('',#3076,#3074,#483,.T.);
#3958=EDGE_CURVE('',#3077,#3078,#1946,.T.);
#3959=EDGE_CURVE('',#3077,#3075,#484,.T.);
#3960=EDGE_CURVE('',#3078,#3076,#485,.T.);
#3961=EDGE_CURVE('',#3079,#3080,#1947,.T.);
#3962=EDGE_CURVE('',#3079,#3077,#486,.T.);
#3963=EDGE_CURVE('',#3080,#3078,#487,.T.);
#3964=EDGE_CURVE('',#3081,#3082,#1948,.T.);
#3965=EDGE_CURVE('',#3081,#3079,#488,.T.);
#3966=EDGE_CURVE('',#3082,#3080,#489,.T.);
#3967=EDGE_CURVE('',#3083,#3084,#1949,.T.);
#3968=EDGE_CURVE('',#3083,#3081,#490,.T.);
#3969=EDGE_CURVE('',#3084,#3082,#491,.T.);
#3970=EDGE_CURVE('',#3026,#3085,#492,.T.);
#3971=EDGE_CURVE('',#3086,#3025,#493,.T.);
#3972=EDGE_CURVE('',#3087,#3086,#2539,.T.);
#3973=EDGE_CURVE('',#3085,#3087,#494,.T.);
#3974=EDGE_CURVE('',#3085,#3088,#1950,.T.);
#3975=EDGE_CURVE('',#3088,#3088,#2540,.T.);
#3976=EDGE_CURVE('',#3089,#3083,#495,.T.);
#3977=EDGE_CURVE('',#2963,#3089,#496,.T.);
#3978=EDGE_CURVE('',#3086,#3021,#497,.T.);
#3979=EDGE_CURVE('',#3090,#3084,#498,.T.);
#3980=EDGE_CURVE('',#3089,#3090,#2541,.T.);
#3981=EDGE_CURVE('',#3022,#3087,#499,.T.);
#3982=EDGE_CURVE('',#3090,#2964,#500,.T.);
#3983=EDGE_CURVE('',#3091,#3092,#1951,.T.);
#3984=EDGE_CURVE('',#3091,#3093,#1952,.T.);
#3985=EDGE_CURVE('',#3093,#3094,#1953,.T.);
#3986=EDGE_CURVE('',#3092,#3094,#1954,.T.);
#3987=EDGE_CURVE('',#3095,#3091,#1955,.T.);
#3988=EDGE_CURVE('',#3095,#3096,#1956,.T.);
#3989=EDGE_CURVE('',#3096,#3093,#1957,.T.);
#3990=EDGE_CURVE('',#3097,#3095,#1958,.T.);
#3991=EDGE_CURVE('',#3097,#3098,#1959,.T.);
#3992=EDGE_CURVE('',#3098,#3096,#1960,.T.);
#3993=EDGE_CURVE('',#3099,#3097,#1961,.T.);
#3994=EDGE_CURVE('',#3099,#3100,#1962,.T.);
#3995=EDGE_CURVE('',#3100,#3098,#1963,.T.);
#3996=EDGE_CURVE('',#3101,#3099,#1964,.T.);
#3997=EDGE_CURVE('',#3101,#3102,#1965,.T.);
#3998=EDGE_CURVE('',#3102,#3100,#1966,.T.);
#3999=EDGE_CURVE('',#3092,#3101,#1967,.T.);
#4000=EDGE_CURVE('',#3094,#3102,#1968,.T.);
#4001=EDGE_CURVE('',#3103,#3103,#2542,.T.);
#4002=EDGE_CURVE('',#3103,#3104,#1969,.T.);
#4003=EDGE_CURVE('',#3104,#3104,#2543,.T.);
#4004=EDGE_CURVE('',#3105,#3106,#1970,.T.);
#4005=EDGE_CURVE('',#3107,#3106,#2544,.F.);
#4006=EDGE_CURVE('',#3107,#3105,#501,.T.);
#4007=EDGE_CURVE('',#3108,#3109,#1971,.T.);
#4008=EDGE_CURVE('',#3109,#3110,#502,.T.);
#4009=EDGE_CURVE('',#3106,#3110,#2545,.F.);
#4010=EDGE_CURVE('',#3105,#3108,#503,.T.);
#4011=EDGE_CURVE('',#3111,#3112,#1972,.T.);
#4012=EDGE_CURVE('',#3112,#3109,#504,.T.);
#4013=EDGE_CURVE('',#3108,#3111,#505,.T.);
#4014=EDGE_CURVE('',#3113,#3114,#1973,.T.);
#4015=EDGE_CURVE('',#3114,#3112,#506,.T.);
#4016=EDGE_CURVE('',#3111,#3113,#507,.T.);
#4017=EDGE_CURVE('',#3115,#3116,#1974,.T.);
#4018=EDGE_CURVE('',#3115,#3117,#508,.T.);
#4019=EDGE_CURVE('',#3118,#3117,#2546,.T.);
#4020=EDGE_CURVE('',#3118,#3116,#509,.T.);
#4021=EDGE_CURVE('',#3119,#3120,#1975,.T.);
#4022=EDGE_CURVE('',#3120,#3121,#510,.T.);
#4023=EDGE_CURVE('',#3122,#3121,#2547,.T.);
#4024=EDGE_CURVE('',#3119,#3122,#511,.T.);
#4025=EDGE_CURVE('',#3123,#3124,#1976,.T.);
#4026=EDGE_CURVE('',#3124,#3120,#512,.T.);
#4027=EDGE_CURVE('',#3123,#3119,#513,.T.);
#4028=EDGE_CURVE('',#3125,#3126,#1977,.T.);
#4029=EDGE_CURVE('',#3126,#3124,#514,.T.);
#4030=EDGE_CURVE('',#3125,#3123,#515,.T.);
#4031=EDGE_CURVE('',#3127,#3128,#1978,.T.);
#4032=EDGE_CURVE('',#3128,#3126,#516,.T.);
#4033=EDGE_CURVE('',#3127,#3125,#517,.T.);
#4034=EDGE_CURVE('',#3129,#3130,#1979,.T.);
#4035=EDGE_CURVE('',#3131,#3129,#518,.T.);
#4036=EDGE_CURVE('',#3132,#3131,#2548,.T.);
#4037=EDGE_CURVE('',#3132,#3130,#519,.T.);
#4038=EDGE_CURVE('',#3130,#3128,#520,.T.);
#4039=EDGE_CURVE('',#3129,#3127,#521,.T.);
#4040=EDGE_CURVE('',#3121,#3107,#522,.T.);
#4041=EDGE_CURVE('',#3117,#3132,#523,.T.);
#4042=EDGE_CURVE('',#3113,#3115,#524,.T.);
#4043=EDGE_CURVE('',#3110,#3122,#525,.T.);
#4044=EDGE_CURVE('',#3116,#3114,#526,.T.);
#4045=EDGE_CURVE('',#3131,#3118,#527,.T.);
#4046=EDGE_CURVE('',#3133,#3134,#1980,.T.);
#4047=EDGE_CURVE('',#3134,#3135,#1981,.T.);
#4048=EDGE_CURVE('',#3135,#3136,#1982,.T.);
#4049=EDGE_CURVE('',#3136,#3137,#1983,.T.);
#4050=EDGE_CURVE('',#3137,#3138,#1984,.T.);
#4051=EDGE_CURVE('',#3138,#3133,#1985,.T.);
#4052=EDGE_CURVE('',#3139,#3140,#1986,.T.);
#4053=EDGE_CURVE('',#3140,#3133,#1987,.T.);
#4054=EDGE_CURVE('',#3139,#3138,#1988,.T.);
#4055=EDGE_CURVE('',#3141,#3139,#1989,.T.);
#4056=EDGE_CURVE('',#3141,#3137,#1990,.T.);
#4057=EDGE_CURVE('',#3142,#3141,#1991,.T.);
#4058=EDGE_CURVE('',#3142,#3136,#1992,.T.);
#4059=EDGE_CURVE('',#3143,#3142,#1993,.T.);
#4060=EDGE_CURVE('',#3143,#3135,#1994,.T.);
#4061=EDGE_CURVE('',#3144,#3143,#1995,.T.);
#4062=EDGE_CURVE('',#3144,#3134,#1996,.T.);
#4063=EDGE_CURVE('',#3140,#3144,#1997,.T.);
#4064=EDGE_CURVE('',#3145,#3145,#2549,.T.);
#4065=EDGE_CURVE('',#3145,#3146,#1998,.T.);
#4066=EDGE_CURVE('',#3146,#3146,#2550,.T.);
#4067=EDGE_CURVE('',#3147,#3147,#2551,.T.);
#4068=EDGE_CURVE('',#3147,#3148,#1999,.T.);
#4069=EDGE_CURVE('',#3148,#3148,#2552,.T.);
#4070=EDGE_CURVE('',#3149,#3149,#2553,.T.);
#4071=EDGE_CURVE('',#3150,#3150,#2554,.T.);
#4072=EDGE_CURVE('',#3151,#3151,#2555,.T.);
#4073=EDGE_CURVE('',#3151,#3149,#2000,.T.);
#4074=EDGE_CURVE('',#3152,#3152,#2556,.T.);
#4075=EDGE_CURVE('',#3153,#3153,#2557,.T.);
#4076=EDGE_CURVE('',#3154,#3154,#2558,.T.);
#4077=EDGE_CURVE('',#3154,#3152,#2001,.T.);
#4078=EDGE_CURVE('',#3155,#3155,#2559,.T.);
#4079=EDGE_CURVE('',#3156,#3156,#2560,.T.);
#4080=EDGE_CURVE('',#3157,#3157,#2561,.T.);
#4081=EDGE_CURVE('',#3157,#3155,#2002,.T.);
#4082=EDGE_CURVE('',#3158,#3158,#2562,.T.);
#4083=EDGE_CURVE('',#3159,#3159,#2563,.T.);
#4084=EDGE_CURVE('',#3160,#3160,#2564,.T.);
#4085=EDGE_CURVE('',#3160,#3158,#2003,.T.);
#4086=EDGE_CURVE('',#3150,#3161,#2004,.T.);
#4087=EDGE_CURVE('',#3161,#3161,#2565,.T.);
#4088=EDGE_CURVE('',#3153,#3162,#2005,.T.);
#4089=EDGE_CURVE('',#3162,#3162,#2566,.T.);
#4090=EDGE_CURVE('',#3156,#3163,#2006,.T.);
#4091=EDGE_CURVE('',#3163,#3163,#2567,.T.);
#4092=EDGE_CURVE('',#3159,#3164,#2007,.T.);
#4093=EDGE_CURVE('',#3164,#3164,#2568,.T.);
#4094=EDGE_CURVE('',#3165,#3166,#2569,.T.);
#4095=EDGE_CURVE('',#3166,#3167,#528,.T.);
#4096=EDGE_CURVE('',#3167,#3168,#2570,.T.);
#4097=EDGE_CURVE('',#3168,#3165,#529,.T.);
#4098=EDGE_CURVE('',#3169,#3170,#2571,.T.);
#4099=EDGE_CURVE('',#3170,#3166,#2008,.T.);
#4100=EDGE_CURVE('',#3165,#3169,#2009,.T.);
#4101=EDGE_CURVE('',#3171,#3172,#2572,.T.);
#4102=EDGE_CURVE('',#3172,#3170,#530,.T.);
#4103=EDGE_CURVE('',#3169,#3171,#531,.T.);
#4104=EDGE_CURVE('',#3173,#3174,#2573,.T.);
#4105=EDGE_CURVE('',#3174,#3172,#532,.T.);
#4106=EDGE_CURVE('',#3171,#3173,#533,.T.);
#4107=EDGE_CURVE('',#3175,#3176,#2574,.T.);
#4108=EDGE_CURVE('',#3176,#3174,#534,.T.);
#4109=EDGE_CURVE('',#3173,#3175,#535,.T.);
#4110=EDGE_CURVE('',#3177,#3178,#2575,.T.);
#4111=EDGE_CURVE('',#3178,#3176,#2010,.T.);
#4112=EDGE_CURVE('',#3175,#3177,#2011,.T.);
#4113=EDGE_CURVE('',#3179,#3180,#2576,.T.);
#4114=EDGE_CURVE('',#3180,#3178,#536,.T.);
#4115=EDGE_CURVE('',#3177,#3179,#537,.T.);
#4116=EDGE_CURVE('',#3167,#3180,#538,.T.);
#4117=EDGE_CURVE('',#3179,#3168,#539,.T.);
#4118=EDGE_CURVE('',#3181,#3178,#540,.T.);
#4119=EDGE_CURVE('',#3182,#3181,#2012,.T.);
#4120=EDGE_CURVE('',#3176,#3182,#541,.T.);
#4121=EDGE_CURVE('',#3180,#3183,#542,.T.);
#4122=EDGE_CURVE('',#3183,#3181,#543,.T.);
#4123=EDGE_CURVE('',#3184,#3167,#544,.T.);
#4124=EDGE_CURVE('',#3183,#3184,#545,.T.);
#4125=EDGE_CURVE('',#3166,#3185,#546,.T.);
#4126=EDGE_CURVE('',#3185,#3184,#547,.T.);
#4127=EDGE_CURVE('',#3186,#3170,#548,.T.);
#4128=EDGE_CURVE('',#3185,#3186,#2013,.T.);
#4129=EDGE_CURVE('',#3182,#3187,#549,.T.);
#4130=EDGE_CURVE('',#3187,#3174,#550,.T.);
#4131=EDGE_CURVE('',#3172,#3188,#551,.T.);
#4132=EDGE_CURVE('',#3188,#3186,#552,.T.);
#4133=EDGE_CURVE('',#3188,#3187,#553,.T.);
#4134=EDGE_CURVE('',#3189,#3189,#2577,.T.);
#4135=EDGE_CURVE('',#3189,#3190,#2014,.T.);
#4136=EDGE_CURVE('',#3190,#3190,#2578,.T.);
#4137=EDGE_CURVE('',#3191,#3191,#2579,.T.);
#4138=EDGE_CURVE('',#3191,#3192,#2015,.T.);
#4139=EDGE_CURVE('',#3192,#3192,#2580,.T.);
#4140=ORIENTED_EDGE('',*,*,#3193,.F.);
#4141=ORIENTED_EDGE('',*,*,#3194,.T.);
#4142=ORIENTED_EDGE('',*,*,#3195,.F.);
#4143=ORIENTED_EDGE('',*,*,#3194,.F.);
#4144=ORIENTED_EDGE('',*,*,#3196,.F.);
#4145=ORIENTED_EDGE('',*,*,#3197,.T.);
#4146=ORIENTED_EDGE('',*,*,#3198,.F.);
#4147=ORIENTED_EDGE('',*,*,#3197,.F.);
#4148=ORIENTED_EDGE('',*,*,#3199,.F.);
#4149=ORIENTED_EDGE('',*,*,#3200,.T.);
#4150=ORIENTED_EDGE('',*,*,#3201,.F.);
#4151=ORIENTED_EDGE('',*,*,#3200,.F.);
#4152=ORIENTED_EDGE('',*,*,#3202,.F.);
#4153=ORIENTED_EDGE('',*,*,#3203,.F.);
#4154=ORIENTED_EDGE('',*,*,#3204,.T.);
#4155=ORIENTED_EDGE('',*,*,#3205,.F.);
#4156=ORIENTED_EDGE('',*,*,#3206,.F.);
#4157=ORIENTED_EDGE('',*,*,#3207,.F.);
#4158=ORIENTED_EDGE('',*,*,#3203,.T.);
#4159=ORIENTED_EDGE('',*,*,#3208,.F.);
#4160=ORIENTED_EDGE('',*,*,#3209,.F.);
#4161=ORIENTED_EDGE('',*,*,#3210,.F.);
#4162=ORIENTED_EDGE('',*,*,#3211,.F.);
#4163=ORIENTED_EDGE('',*,*,#3206,.T.);
#4164=ORIENTED_EDGE('',*,*,#3210,.T.);
#4165=ORIENTED_EDGE('',*,*,#3212,.T.);
#4166=ORIENTED_EDGE('',*,*,#3213,.T.);
#4167=ORIENTED_EDGE('',*,*,#3202,.T.);
#4168=ORIENTED_EDGE('',*,*,#3214,.T.);
#4169=ORIENTED_EDGE('',*,*,#3215,.F.);
#4170=ORIENTED_EDGE('',*,*,#3216,.T.);
#4171=ORIENTED_EDGE('',*,*,#3217,.T.);
#4172=ORIENTED_EDGE('',*,*,#3218,.T.);
#4173=ORIENTED_EDGE('',*,*,#3208,.T.);
#4174=ORIENTED_EDGE('',*,*,#3219,.F.);
#4175=ORIENTED_EDGE('',*,*,#3220,.F.);
#4176=ORIENTED_EDGE('',*,*,#3221,.T.);
#4177=ORIENTED_EDGE('',*,*,#3216,.F.);
#4178=ORIENTED_EDGE('',*,*,#3222,.F.);
#4179=ORIENTED_EDGE('',*,*,#3214,.F.);
#4180=ORIENTED_EDGE('',*,*,#3204,.F.);
#4181=ORIENTED_EDGE('',*,*,#3223,.F.);
#4182=ORIENTED_EDGE('',*,*,#3224,.F.);
#4183=ORIENTED_EDGE('',*,*,#3211,.T.);
#4184=ORIENTED_EDGE('',*,*,#3213,.F.);
#4185=ORIENTED_EDGE('',*,*,#3225,.F.);
#4186=ORIENTED_EDGE('',*,*,#3205,.T.);
#4187=ORIENTED_EDGE('',*,*,#3218,.F.);
#4188=ORIENTED_EDGE('',*,*,#3226,.F.);
#4189=ORIENTED_EDGE('',*,*,#3227,.F.);
#4190=ORIENTED_EDGE('',*,*,#3225,.T.);
#4191=ORIENTED_EDGE('',*,*,#3212,.F.);
#4192=ORIENTED_EDGE('',*,*,#3209,.T.);
#4193=ORIENTED_EDGE('',*,*,#3228,.F.);
#4194=ORIENTED_EDGE('',*,*,#3226,.T.);
#4195=ORIENTED_EDGE('',*,*,#3217,.F.);
#4196=ORIENTED_EDGE('',*,*,#3221,.F.);
#4197=ORIENTED_EDGE('',*,*,#3229,.T.);
#4198=ORIENTED_EDGE('',*,*,#3230,.T.);
#4199=ORIENTED_EDGE('',*,*,#3231,.T.);
#4200=ORIENTED_EDGE('',*,*,#3232,.F.);
#4201=ORIENTED_EDGE('',*,*,#3233,.F.);
#4202=ORIENTED_EDGE('',*,*,#3234,.F.);
#4203=ORIENTED_EDGE('',*,*,#3235,.F.);
#4204=ORIENTED_EDGE('',*,*,#3236,.F.);
#4205=ORIENTED_EDGE('',*,*,#3237,.F.);
#4206=ORIENTED_EDGE('',*,*,#3238,.F.);
#4207=ORIENTED_EDGE('',*,*,#3239,.F.);
#4208=ORIENTED_EDGE('',*,*,#3240,.T.);
#4209=ORIENTED_EDGE('',*,*,#3241,.T.);
#4210=ORIENTED_EDGE('',*,*,#3223,.T.);
#4211=ORIENTED_EDGE('',*,*,#3207,.T.);
#4212=ORIENTED_EDGE('',*,*,#3224,.T.);
#4213=ORIENTED_EDGE('',*,*,#3227,.T.);
#4214=ORIENTED_EDGE('',*,*,#3228,.T.);
#4215=ORIENTED_EDGE('',*,*,#3220,.T.);
#4216=ORIENTED_EDGE('',*,*,#3195,.T.);
#4217=ORIENTED_EDGE('',*,*,#3198,.T.);
#4218=ORIENTED_EDGE('',*,*,#3201,.T.);
#4219=ORIENTED_EDGE('',*,*,#3242,.F.);
#4220=ORIENTED_EDGE('',*,*,#3243,.F.);
#4221=ORIENTED_EDGE('',*,*,#3244,.F.);
#4222=ORIENTED_EDGE('',*,*,#3240,.F.);
#4223=ORIENTED_EDGE('',*,*,#3222,.T.);
#4224=ORIENTED_EDGE('',*,*,#3241,.F.);
#4225=ORIENTED_EDGE('',*,*,#3244,.T.);
#4226=ORIENTED_EDGE('',*,*,#3245,.F.);
#4227=ORIENTED_EDGE('',*,*,#3246,.F.);
#4228=ORIENTED_EDGE('',*,*,#3229,.F.);
#4229=ORIENTED_EDGE('',*,*,#3219,.T.);
#4230=ORIENTED_EDGE('',*,*,#3215,.T.);
#4231=ORIENTED_EDGE('',*,*,#3230,.F.);
#4232=ORIENTED_EDGE('',*,*,#3246,.T.);
#4233=ORIENTED_EDGE('',*,*,#3247,.F.);
#4234=ORIENTED_EDGE('',*,*,#3248,.F.);
#4235=ORIENTED_EDGE('',*,*,#3249,.F.);
#4236=ORIENTED_EDGE('',*,*,#3231,.F.);
#4237=ORIENTED_EDGE('',*,*,#3248,.T.);
#4238=ORIENTED_EDGE('',*,*,#3250,.F.);
#4239=ORIENTED_EDGE('',*,*,#3242,.T.);
#4240=ORIENTED_EDGE('',*,*,#3239,.T.);
#4241=ORIENTED_EDGE('',*,*,#3251,.T.);
#4242=ORIENTED_EDGE('',*,*,#3252,.F.);
#4243=ORIENTED_EDGE('',*,*,#3249,.T.);
#4244=ORIENTED_EDGE('',*,*,#3253,.F.);
#4245=ORIENTED_EDGE('',*,*,#3254,.T.);
#4246=ORIENTED_EDGE('',*,*,#3232,.T.);
#4247=ORIENTED_EDGE('',*,*,#3252,.T.);
#4248=ORIENTED_EDGE('',*,*,#3255,.T.);
#4249=ORIENTED_EDGE('',*,*,#3256,.T.);
#4250=ORIENTED_EDGE('',*,*,#3257,.T.);
#4251=ORIENTED_EDGE('',*,*,#3258,.T.);
#4252=ORIENTED_EDGE('',*,*,#3259,.T.);
#4253=ORIENTED_EDGE('',*,*,#3260,.T.);
#4254=ORIENTED_EDGE('',*,*,#3253,.T.);
#4255=ORIENTED_EDGE('',*,*,#3250,.T.);
#4256=ORIENTED_EDGE('',*,*,#3247,.T.);
#4257=ORIENTED_EDGE('',*,*,#3245,.T.);
#4258=ORIENTED_EDGE('',*,*,#3243,.T.);
#4259=ORIENTED_EDGE('',*,*,#3193,.T.);
#4260=ORIENTED_EDGE('',*,*,#3196,.T.);
#4261=ORIENTED_EDGE('',*,*,#3199,.T.);
#4262=ORIENTED_EDGE('',*,*,#3251,.F.);
#4263=ORIENTED_EDGE('',*,*,#3238,.T.);
#4264=ORIENTED_EDGE('',*,*,#3261,.T.);
#4265=ORIENTED_EDGE('',*,*,#3255,.F.);
#4266=ORIENTED_EDGE('',*,*,#3254,.F.);
#4267=ORIENTED_EDGE('',*,*,#3260,.F.);
#4268=ORIENTED_EDGE('',*,*,#3262,.F.);
#4269=ORIENTED_EDGE('',*,*,#3233,.T.);
#4270=ORIENTED_EDGE('',*,*,#3234,.T.);
#4271=ORIENTED_EDGE('',*,*,#3262,.T.);
#4272=ORIENTED_EDGE('',*,*,#3259,.F.);
#4273=ORIENTED_EDGE('',*,*,#3263,.F.);
#4274=ORIENTED_EDGE('',*,*,#3235,.T.);
#4275=ORIENTED_EDGE('',*,*,#3263,.T.);
#4276=ORIENTED_EDGE('',*,*,#3258,.F.);
#4277=ORIENTED_EDGE('',*,*,#3264,.F.);
#4278=ORIENTED_EDGE('',*,*,#3236,.T.);
#4279=ORIENTED_EDGE('',*,*,#3264,.T.);
#4280=ORIENTED_EDGE('',*,*,#3257,.F.);
#4281=ORIENTED_EDGE('',*,*,#3265,.F.);
#4282=ORIENTED_EDGE('',*,*,#3237,.T.);
#4283=ORIENTED_EDGE('',*,*,#3265,.T.);
#4284=ORIENTED_EDGE('',*,*,#3256,.F.);
#4285=ORIENTED_EDGE('',*,*,#3261,.F.);
#4286=ORIENTED_EDGE('',*,*,#3266,.T.);
#4287=ORIENTED_EDGE('',*,*,#3267,.T.);
#4288=ORIENTED_EDGE('',*,*,#3268,.F.);
#4289=ORIENTED_EDGE('',*,*,#3267,.F.);
#4290=ORIENTED_EDGE('',*,*,#3269,.F.);
#4291=ORIENTED_EDGE('',*,*,#3266,.F.);
#4292=ORIENTED_EDGE('',*,*,#3270,.F.);
#4293=ORIENTED_EDGE('',*,*,#3268,.T.);
#4294=ORIENTED_EDGE('',*,*,#3271,.F.);
#4295=ORIENTED_EDGE('',*,*,#3272,.T.);
#4296=ORIENTED_EDGE('',*,*,#3270,.T.);
#4297=ORIENTED_EDGE('',*,*,#3272,.F.);
#4298=ORIENTED_EDGE('',*,*,#3273,.T.);
#4299=ORIENTED_EDGE('',*,*,#3274,.F.);
#4300=ORIENTED_EDGE('',*,*,#3273,.F.);
#4301=ORIENTED_EDGE('',*,*,#3275,.T.);
#4302=ORIENTED_EDGE('',*,*,#3276,.T.);
#4303=ORIENTED_EDGE('',*,*,#3275,.F.);
#4304=ORIENTED_EDGE('',*,*,#3276,.F.);
#4305=ORIENTED_EDGE('',*,*,#3269,.T.);
#4306=ORIENTED_EDGE('',*,*,#3277,.T.);
#4307=ORIENTED_EDGE('',*,*,#3274,.T.);
#4308=ORIENTED_EDGE('',*,*,#3277,.F.);
#4309=ORIENTED_EDGE('',*,*,#3271,.T.);
#4310=ORIENTED_EDGE('',*,*,#3278,.F.);
#4311=ORIENTED_EDGE('',*,*,#3279,.F.);
#4312=ORIENTED_EDGE('',*,*,#3280,.F.);
#4313=ORIENTED_EDGE('',*,*,#3281,.F.);
#4314=ORIENTED_EDGE('',*,*,#3282,.F.);
#4315=ORIENTED_EDGE('',*,*,#3283,.F.);
#4316=ORIENTED_EDGE('',*,*,#3284,.F.);
#4317=ORIENTED_EDGE('',*,*,#3285,.F.);
#4318=ORIENTED_EDGE('',*,*,#3285,.T.);
#4319=ORIENTED_EDGE('',*,*,#3286,.F.);
#4320=ORIENTED_EDGE('',*,*,#3279,.T.);
#4321=ORIENTED_EDGE('',*,*,#3287,.F.);
#4322=ORIENTED_EDGE('',*,*,#3282,.T.);
#4323=ORIENTED_EDGE('',*,*,#3287,.T.);
#4324=ORIENTED_EDGE('',*,*,#3278,.T.);
#4325=ORIENTED_EDGE('',*,*,#3288,.F.);
#4326=ORIENTED_EDGE('',*,*,#3284,.T.);
#4327=ORIENTED_EDGE('',*,*,#3289,.F.);
#4328=ORIENTED_EDGE('',*,*,#3280,.T.);
#4329=ORIENTED_EDGE('',*,*,#3286,.T.);
#4330=ORIENTED_EDGE('',*,*,#3283,.T.);
#4331=ORIENTED_EDGE('',*,*,#3288,.T.);
#4332=ORIENTED_EDGE('',*,*,#3281,.T.);
#4333=ORIENTED_EDGE('',*,*,#3289,.T.);
#4334=ORIENTED_EDGE('',*,*,#3290,.F.);
#4335=ORIENTED_EDGE('',*,*,#3291,.T.);
#4336=ORIENTED_EDGE('',*,*,#3292,.F.);
#4337=ORIENTED_EDGE('',*,*,#3293,.T.);
#4338=ORIENTED_EDGE('',*,*,#3294,.F.);
#4339=ORIENTED_EDGE('',*,*,#3295,.T.);
#4340=ORIENTED_EDGE('',*,*,#3296,.F.);
#4341=ORIENTED_EDGE('',*,*,#3297,.T.);
#4342=ORIENTED_EDGE('',*,*,#3292,.T.);
#4343=ORIENTED_EDGE('',*,*,#3298,.F.);
#4344=ORIENTED_EDGE('',*,*,#3299,.T.);
#4345=ORIENTED_EDGE('',*,*,#3300,.F.);
#4346=ORIENTED_EDGE('',*,*,#3301,.T.);
#4347=ORIENTED_EDGE('',*,*,#3302,.F.);
#4348=ORIENTED_EDGE('',*,*,#3296,.T.);
#4349=ORIENTED_EDGE('',*,*,#3303,.F.);
#4350=ORIENTED_EDGE('',*,*,#3304,.T.);
#4351=ORIENTED_EDGE('',*,*,#3305,.F.);
#4352=ORIENTED_EDGE('',*,*,#3306,.T.);
#4353=ORIENTED_EDGE('',*,*,#3307,.F.);
#4354=ORIENTED_EDGE('',*,*,#3308,.T.);
#4355=ORIENTED_EDGE('',*,*,#3309,.T.);
#4356=ORIENTED_EDGE('',*,*,#3303,.T.);
#4357=ORIENTED_EDGE('',*,*,#3297,.F.);
#4358=ORIENTED_EDGE('',*,*,#3307,.T.);
#4359=ORIENTED_EDGE('',*,*,#3310,.T.);
#4360=ORIENTED_EDGE('',*,*,#3311,.T.);
#4361=ORIENTED_EDGE('',*,*,#3291,.F.);
#4362=ORIENTED_EDGE('',*,*,#3312,.T.);
#4363=ORIENTED_EDGE('',*,*,#3313,.T.);
#4364=ORIENTED_EDGE('',*,*,#3314,.T.);
#4365=ORIENTED_EDGE('',*,*,#3315,.F.);
#4366=ORIENTED_EDGE('',*,*,#3316,.T.);
#4367=ORIENTED_EDGE('',*,*,#3312,.F.);
#4368=ORIENTED_EDGE('',*,*,#3316,.F.);
#4369=ORIENTED_EDGE('',*,*,#3317,.F.);
#4370=ORIENTED_EDGE('',*,*,#3318,.T.);
#4371=ORIENTED_EDGE('',*,*,#3319,.F.);
#4372=ORIENTED_EDGE('',*,*,#3318,.F.);
#4373=ORIENTED_EDGE('',*,*,#3320,.F.);
#4374=ORIENTED_EDGE('',*,*,#3321,.T.);
#4375=ORIENTED_EDGE('',*,*,#3322,.F.);
#4376=ORIENTED_EDGE('',*,*,#3321,.F.);
#4377=ORIENTED_EDGE('',*,*,#3323,.F.);
#4378=ORIENTED_EDGE('',*,*,#3324,.T.);
#4379=ORIENTED_EDGE('',*,*,#3313,.F.);
#4380=ORIENTED_EDGE('',*,*,#3324,.F.);
#4381=ORIENTED_EDGE('',*,*,#3325,.F.);
#4382=ORIENTED_EDGE('',*,*,#3326,.T.);
#4383=ORIENTED_EDGE('',*,*,#3327,.T.);
#4384=ORIENTED_EDGE('',*,*,#3326,.F.);
#4385=ORIENTED_EDGE('',*,*,#3327,.F.);
#4386=ORIENTED_EDGE('',*,*,#3328,.F.);
#4387=ORIENTED_EDGE('',*,*,#3329,.F.);
#4388=ORIENTED_EDGE('',*,*,#3330,.T.);
#4389=ORIENTED_EDGE('',*,*,#3331,.T.);
#4390=ORIENTED_EDGE('',*,*,#3330,.F.);
#4391=ORIENTED_EDGE('',*,*,#3331,.F.);
#4392=ORIENTED_EDGE('',*,*,#3332,.F.);
#4393=ORIENTED_EDGE('',*,*,#3328,.T.);
#4394=ORIENTED_EDGE('',*,*,#3333,.T.);
#4395=ORIENTED_EDGE('',*,*,#3334,.F.);
#4396=ORIENTED_EDGE('',*,*,#3333,.F.);
#4397=ORIENTED_EDGE('',*,*,#3332,.T.);
#4398=ORIENTED_EDGE('',*,*,#3335,.T.);
#4399=ORIENTED_EDGE('',*,*,#3336,.F.);
#4400=ORIENTED_EDGE('',*,*,#3335,.F.);
#4401=ORIENTED_EDGE('',*,*,#3337,.F.);
#4402=ORIENTED_EDGE('',*,*,#3338,.F.);
#4403=ORIENTED_EDGE('',*,*,#3339,.F.);
#4404=ORIENTED_EDGE('',*,*,#3340,.T.);
#4405=ORIENTED_EDGE('',*,*,#3341,.F.);
#4406=ORIENTED_EDGE('',*,*,#3342,.T.);
#4407=ORIENTED_EDGE('',*,*,#3343,.F.);
#4408=ORIENTED_EDGE('',*,*,#3344,.F.);
#4409=ORIENTED_EDGE('',*,*,#3345,.F.);
#4410=ORIENTED_EDGE('',*,*,#3346,.T.);
#4411=ORIENTED_EDGE('',*,*,#3347,.F.);
#4412=ORIENTED_EDGE('',*,*,#3348,.F.);
#4413=ORIENTED_EDGE('',*,*,#3349,.F.);
#4414=ORIENTED_EDGE('',*,*,#3350,.T.);
#4415=ORIENTED_EDGE('',*,*,#3351,.F.);
#4416=ORIENTED_EDGE('',*,*,#3352,.F.);
#4417=ORIENTED_EDGE('',*,*,#3353,.F.);
#4418=ORIENTED_EDGE('',*,*,#3354,.T.);
#4419=ORIENTED_EDGE('',*,*,#3355,.F.);
#4420=ORIENTED_EDGE('',*,*,#3356,.F.);
#4421=ORIENTED_EDGE('',*,*,#3357,.F.);
#4422=ORIENTED_EDGE('',*,*,#3358,.F.);
#4423=ORIENTED_EDGE('',*,*,#3359,.F.);
#4424=ORIENTED_EDGE('',*,*,#3360,.T.);
#4425=ORIENTED_EDGE('',*,*,#3361,.F.);
#4426=ORIENTED_EDGE('',*,*,#3362,.F.);
#4427=ORIENTED_EDGE('',*,*,#3363,.F.);
#4428=ORIENTED_EDGE('',*,*,#3364,.T.);
#4429=ORIENTED_EDGE('',*,*,#3365,.F.);
#4430=ORIENTED_EDGE('',*,*,#3334,.T.);
#4431=ORIENTED_EDGE('',*,*,#3366,.F.);
#4432=ORIENTED_EDGE('',*,*,#3336,.T.);
#4433=ORIENTED_EDGE('',*,*,#3367,.F.);
#4434=ORIENTED_EDGE('',*,*,#3340,.F.);
#4435=ORIENTED_EDGE('',*,*,#3368,.F.);
#4436=ORIENTED_EDGE('',*,*,#3354,.F.);
#4437=ORIENTED_EDGE('',*,*,#3369,.F.);
#4438=ORIENTED_EDGE('',*,*,#3360,.F.);
#4439=ORIENTED_EDGE('',*,*,#3370,.F.);
#4440=ORIENTED_EDGE('',*,*,#3342,.F.);
#4441=ORIENTED_EDGE('',*,*,#3371,.F.);
#4442=ORIENTED_EDGE('',*,*,#3364,.F.);
#4443=ORIENTED_EDGE('',*,*,#3372,.F.);
#4444=ORIENTED_EDGE('',*,*,#3346,.F.);
#4445=ORIENTED_EDGE('',*,*,#3373,.F.);
#4446=ORIENTED_EDGE('',*,*,#3374,.F.);
#4447=ORIENTED_EDGE('',*,*,#3375,.F.);
#4448=ORIENTED_EDGE('',*,*,#3350,.F.);
#4449=ORIENTED_EDGE('',*,*,#3376,.F.);
#4450=ORIENTED_EDGE('',*,*,#3377,.F.);
#4451=ORIENTED_EDGE('',*,*,#3378,.F.);
#4452=ORIENTED_EDGE('',*,*,#3374,.T.);
#4453=ORIENTED_EDGE('',*,*,#3379,.T.);
#4454=ORIENTED_EDGE('',*,*,#3380,.F.);
#4455=ORIENTED_EDGE('',*,*,#3381,.F.);
#4456=ORIENTED_EDGE('',*,*,#3310,.F.);
#4457=ORIENTED_EDGE('',*,*,#3306,.F.);
#4458=ORIENTED_EDGE('',*,*,#3382,.F.);
#4459=ORIENTED_EDGE('',*,*,#3351,.T.);
#4460=ORIENTED_EDGE('',*,*,#3375,.T.);
#4461=ORIENTED_EDGE('',*,*,#3378,.T.);
#4462=ORIENTED_EDGE('',*,*,#3383,.T.);
#4463=ORIENTED_EDGE('',*,*,#3384,.F.);
#4464=ORIENTED_EDGE('',*,*,#3304,.F.);
#4465=ORIENTED_EDGE('',*,*,#3309,.F.);
#4466=ORIENTED_EDGE('',*,*,#3385,.F.);
#4467=ORIENTED_EDGE('',*,*,#3386,.F.);
#4468=ORIENTED_EDGE('',*,*,#3387,.T.);
#4469=ORIENTED_EDGE('',*,*,#3347,.T.);
#4470=ORIENTED_EDGE('',*,*,#3372,.T.);
#4471=ORIENTED_EDGE('',*,*,#3363,.T.);
#4472=ORIENTED_EDGE('',*,*,#3388,.T.);
#4473=ORIENTED_EDGE('',*,*,#3389,.F.);
#4474=ORIENTED_EDGE('',*,*,#3390,.F.);
#4475=ORIENTED_EDGE('',*,*,#3391,.F.);
#4476=ORIENTED_EDGE('',*,*,#3392,.F.);
#4477=ORIENTED_EDGE('',*,*,#3393,.F.);
#4478=ORIENTED_EDGE('',*,*,#3394,.T.);
#4479=ORIENTED_EDGE('',*,*,#3343,.T.);
#4480=ORIENTED_EDGE('',*,*,#3370,.T.);
#4481=ORIENTED_EDGE('',*,*,#3359,.T.);
#4482=ORIENTED_EDGE('',*,*,#3395,.T.);
#4483=ORIENTED_EDGE('',*,*,#3396,.F.);
#4484=ORIENTED_EDGE('',*,*,#3299,.F.);
#4485=ORIENTED_EDGE('',*,*,#3397,.F.);
#4486=ORIENTED_EDGE('',*,*,#3398,.F.);
#4487=ORIENTED_EDGE('',*,*,#3399,.F.);
#4488=ORIENTED_EDGE('',*,*,#3400,.T.);
#4489=ORIENTED_EDGE('',*,*,#3337,.T.);
#4490=ORIENTED_EDGE('',*,*,#3367,.T.);
#4491=ORIENTED_EDGE('',*,*,#3353,.T.);
#4492=ORIENTED_EDGE('',*,*,#3401,.F.);
#4493=ORIENTED_EDGE('',*,*,#3402,.T.);
#4494=ORIENTED_EDGE('',*,*,#3403,.T.);
#4495=ORIENTED_EDGE('',*,*,#3404,.T.);
#4496=ORIENTED_EDGE('',*,*,#3405,.F.);
#4497=ORIENTED_EDGE('',*,*,#3352,.T.);
#4498=ORIENTED_EDGE('',*,*,#3387,.F.);
#4499=ORIENTED_EDGE('',*,*,#3406,.T.);
#4500=ORIENTED_EDGE('',*,*,#3379,.F.);
#4501=ORIENTED_EDGE('',*,*,#3407,.T.);
#4502=ORIENTED_EDGE('',*,*,#3383,.F.);
#4503=ORIENTED_EDGE('',*,*,#3377,.T.);
#4504=ORIENTED_EDGE('',*,*,#3408,.F.);
#4505=ORIENTED_EDGE('',*,*,#3409,.T.);
#4506=ORIENTED_EDGE('',*,*,#3388,.F.);
#4507=ORIENTED_EDGE('',*,*,#3362,.T.);
#4508=ORIENTED_EDGE('',*,*,#3410,.F.);
#4509=ORIENTED_EDGE('',*,*,#3411,.T.);
#4510=ORIENTED_EDGE('',*,*,#3395,.F.);
#4511=ORIENTED_EDGE('',*,*,#3358,.T.);
#4512=ORIENTED_EDGE('',*,*,#3412,.F.);
#4513=ORIENTED_EDGE('',*,*,#3413,.T.);
#4514=ORIENTED_EDGE('',*,*,#3414,.T.);
#4515=ORIENTED_EDGE('',*,*,#3401,.T.);
#4516=ORIENTED_EDGE('',*,*,#3356,.T.);
#4517=ORIENTED_EDGE('',*,*,#3415,.T.);
#4518=ORIENTED_EDGE('',*,*,#3416,.F.);
#4519=ORIENTED_EDGE('',*,*,#3417,.T.);
#4520=ORIENTED_EDGE('',*,*,#3418,.F.);
#4521=ORIENTED_EDGE('',*,*,#3419,.T.);
#4522=ORIENTED_EDGE('',*,*,#3420,.F.);
#4523=ORIENTED_EDGE('',*,*,#3421,.T.);
#4524=ORIENTED_EDGE('',*,*,#3422,.F.);
#4525=ORIENTED_EDGE('',*,*,#3423,.T.);
#4526=ORIENTED_EDGE('',*,*,#3338,.T.);
#4527=ORIENTED_EDGE('',*,*,#3405,.T.);
#4528=ORIENTED_EDGE('',*,*,#3424,.T.);
#4529=ORIENTED_EDGE('',*,*,#3425,.T.);
#4530=ORIENTED_EDGE('',*,*,#3426,.F.);
#4531=ORIENTED_EDGE('',*,*,#3344,.T.);
#4532=ORIENTED_EDGE('',*,*,#3400,.F.);
#4533=ORIENTED_EDGE('',*,*,#3427,.T.);
#4534=ORIENTED_EDGE('',*,*,#3428,.F.);
#4535=ORIENTED_EDGE('',*,*,#3348,.T.);
#4536=ORIENTED_EDGE('',*,*,#3394,.F.);
#4537=ORIENTED_EDGE('',*,*,#3429,.T.);
#4538=ORIENTED_EDGE('',*,*,#3430,.F.);
#4539=ORIENTED_EDGE('',*,*,#3431,.T.);
#4540=ORIENTED_EDGE('',*,*,#3432,.T.);
#4541=ORIENTED_EDGE('',*,*,#3433,.T.);
#4542=ORIENTED_EDGE('',*,*,#3434,.T.);
#4543=ORIENTED_EDGE('',*,*,#3435,.T.);
#4544=ORIENTED_EDGE('',*,*,#3436,.F.);
#4545=ORIENTED_EDGE('',*,*,#3314,.F.);
#4546=ORIENTED_EDGE('',*,*,#3437,.T.);
#4547=ORIENTED_EDGE('',*,*,#3366,.T.);
#4548=ORIENTED_EDGE('',*,*,#3437,.F.);
#4549=ORIENTED_EDGE('',*,*,#3438,.F.);
#4550=ORIENTED_EDGE('',*,*,#3439,.T.);
#4551=ORIENTED_EDGE('',*,*,#3365,.T.);
#4552=ORIENTED_EDGE('',*,*,#3439,.F.);
#4553=ORIENTED_EDGE('',*,*,#3440,.F.);
#4554=ORIENTED_EDGE('',*,*,#3436,.T.);
#4555=ORIENTED_EDGE('',*,*,#3441,.F.);
#4556=ORIENTED_EDGE('',*,*,#3442,.F.);
#4557=ORIENTED_EDGE('',*,*,#3443,.F.);
#4558=ORIENTED_EDGE('',*,*,#3444,.F.);
#4559=ORIENTED_EDGE('',*,*,#3380,.T.);
#4560=ORIENTED_EDGE('',*,*,#3406,.F.);
#4561=ORIENTED_EDGE('',*,*,#3386,.T.);
#4562=ORIENTED_EDGE('',*,*,#3445,.T.);
#4563=ORIENTED_EDGE('',*,*,#3440,.T.);
#4564=ORIENTED_EDGE('',*,*,#3446,.T.);
#4565=ORIENTED_EDGE('',*,*,#3447,.T.);
#4566=ORIENTED_EDGE('',*,*,#3431,.F.);
#4567=ORIENTED_EDGE('',*,*,#3290,.T.);
#4568=ORIENTED_EDGE('',*,*,#3311,.F.);
#4569=ORIENTED_EDGE('',*,*,#3381,.T.);
#4570=ORIENTED_EDGE('',*,*,#3445,.F.);
#4571=ORIENTED_EDGE('',*,*,#3385,.T.);
#4572=ORIENTED_EDGE('',*,*,#3308,.F.);
#4573=ORIENTED_EDGE('',*,*,#3444,.T.);
#4574=ORIENTED_EDGE('',*,*,#3448,.F.);
#4575=ORIENTED_EDGE('',*,*,#3449,.F.);
#4576=ORIENTED_EDGE('',*,*,#3446,.F.);
#4577=ORIENTED_EDGE('',*,*,#3443,.T.);
#4578=ORIENTED_EDGE('',*,*,#3450,.T.);
#4579=ORIENTED_EDGE('',*,*,#3451,.T.);
#4580=ORIENTED_EDGE('',*,*,#3448,.T.);
#4581=ORIENTED_EDGE('',*,*,#3382,.T.);
#4582=ORIENTED_EDGE('',*,*,#3305,.T.);
#4583=ORIENTED_EDGE('',*,*,#3384,.T.);
#4584=ORIENTED_EDGE('',*,*,#3407,.F.);
#4585=ORIENTED_EDGE('',*,*,#3441,.T.);
#4586=ORIENTED_EDGE('',*,*,#3435,.F.);
#4587=ORIENTED_EDGE('',*,*,#3452,.T.);
#4588=ORIENTED_EDGE('',*,*,#3453,.T.);
#4589=ORIENTED_EDGE('',*,*,#3349,.T.);
#4590=ORIENTED_EDGE('',*,*,#3430,.T.);
#4591=ORIENTED_EDGE('',*,*,#3454,.F.);
#4592=ORIENTED_EDGE('',*,*,#3455,.F.);
#4593=ORIENTED_EDGE('',*,*,#3456,.F.);
#4594=ORIENTED_EDGE('',*,*,#3457,.F.);
#4595=ORIENTED_EDGE('',*,*,#3458,.F.);
#4596=ORIENTED_EDGE('',*,*,#3408,.T.);
#4597=ORIENTED_EDGE('',*,*,#3376,.T.);
#4598=ORIENTED_EDGE('',*,*,#3373,.T.);
#4599=ORIENTED_EDGE('',*,*,#3454,.T.);
#4600=ORIENTED_EDGE('',*,*,#3429,.F.);
#4601=ORIENTED_EDGE('',*,*,#3393,.T.);
#4602=ORIENTED_EDGE('',*,*,#3459,.T.);
#4603=ORIENTED_EDGE('',*,*,#3455,.T.);
#4604=ORIENTED_EDGE('',*,*,#3459,.F.);
#4605=ORIENTED_EDGE('',*,*,#3392,.T.);
#4606=ORIENTED_EDGE('',*,*,#3460,.F.);
#4607=ORIENTED_EDGE('',*,*,#3456,.T.);
#4608=ORIENTED_EDGE('',*,*,#3460,.T.);
#4609=ORIENTED_EDGE('',*,*,#3391,.T.);
#4610=ORIENTED_EDGE('',*,*,#3461,.T.);
#4611=ORIENTED_EDGE('',*,*,#3457,.T.);
#4612=ORIENTED_EDGE('',*,*,#3461,.F.);
#4613=ORIENTED_EDGE('',*,*,#3390,.T.);
#4614=ORIENTED_EDGE('',*,*,#3462,.F.);
#4615=ORIENTED_EDGE('',*,*,#3458,.T.);
#4616=ORIENTED_EDGE('',*,*,#3462,.T.);
#4617=ORIENTED_EDGE('',*,*,#3389,.T.);
#4618=ORIENTED_EDGE('',*,*,#3409,.F.);
#4619=ORIENTED_EDGE('',*,*,#3345,.T.);
#4620=ORIENTED_EDGE('',*,*,#3428,.T.);
#4621=ORIENTED_EDGE('',*,*,#3463,.F.);
#4622=ORIENTED_EDGE('',*,*,#3464,.F.);
#4623=ORIENTED_EDGE('',*,*,#3465,.F.);
#4624=ORIENTED_EDGE('',*,*,#3301,.F.);
#4625=ORIENTED_EDGE('',*,*,#3466,.F.);
#4626=ORIENTED_EDGE('',*,*,#3410,.T.);
#4627=ORIENTED_EDGE('',*,*,#3361,.T.);
#4628=ORIENTED_EDGE('',*,*,#3371,.T.);
#4629=ORIENTED_EDGE('',*,*,#3463,.T.);
#4630=ORIENTED_EDGE('',*,*,#3427,.F.);
#4631=ORIENTED_EDGE('',*,*,#3399,.T.);
#4632=ORIENTED_EDGE('',*,*,#3467,.T.);
#4633=ORIENTED_EDGE('',*,*,#3294,.T.);
#4634=ORIENTED_EDGE('',*,*,#3468,.F.);
#4635=ORIENTED_EDGE('',*,*,#3464,.T.);
#4636=ORIENTED_EDGE('',*,*,#3467,.F.);
#4637=ORIENTED_EDGE('',*,*,#3398,.T.);
#4638=ORIENTED_EDGE('',*,*,#3469,.F.);
#4639=ORIENTED_EDGE('',*,*,#3302,.T.);
#4640=ORIENTED_EDGE('',*,*,#3465,.T.);
#4641=ORIENTED_EDGE('',*,*,#3468,.T.);
#4642=ORIENTED_EDGE('',*,*,#3295,.F.);
#4643=ORIENTED_EDGE('',*,*,#3469,.T.);
#4644=ORIENTED_EDGE('',*,*,#3397,.T.);
#4645=ORIENTED_EDGE('',*,*,#3298,.T.);
#4646=ORIENTED_EDGE('',*,*,#3293,.F.);
#4647=ORIENTED_EDGE('',*,*,#3322,.T.);
#4648=ORIENTED_EDGE('',*,*,#3319,.T.);
#4649=ORIENTED_EDGE('',*,*,#3438,.T.);
#4650=ORIENTED_EDGE('',*,*,#3466,.T.);
#4651=ORIENTED_EDGE('',*,*,#3300,.T.);
#4652=ORIENTED_EDGE('',*,*,#3396,.T.);
#4653=ORIENTED_EDGE('',*,*,#3411,.F.);
#4654=ORIENTED_EDGE('',*,*,#3341,.T.);
#4655=ORIENTED_EDGE('',*,*,#3426,.T.);
#4656=ORIENTED_EDGE('',*,*,#3470,.F.);
#4657=ORIENTED_EDGE('',*,*,#3471,.F.);
#4658=ORIENTED_EDGE('',*,*,#3472,.F.);
#4659=ORIENTED_EDGE('',*,*,#3473,.F.);
#4660=ORIENTED_EDGE('',*,*,#3474,.F.);
#4661=ORIENTED_EDGE('',*,*,#3412,.T.);
#4662=ORIENTED_EDGE('',*,*,#3357,.T.);
#4663=ORIENTED_EDGE('',*,*,#3369,.T.);
#4664=ORIENTED_EDGE('',*,*,#3470,.T.);
#4665=ORIENTED_EDGE('',*,*,#3425,.F.);
#4666=ORIENTED_EDGE('',*,*,#3475,.T.);
#4667=ORIENTED_EDGE('',*,*,#3476,.T.);
#4668=ORIENTED_EDGE('',*,*,#3471,.T.);
#4669=ORIENTED_EDGE('',*,*,#3476,.F.);
#4670=ORIENTED_EDGE('',*,*,#3477,.F.);
#4671=ORIENTED_EDGE('',*,*,#3478,.F.);
#4672=ORIENTED_EDGE('',*,*,#3472,.T.);
#4673=ORIENTED_EDGE('',*,*,#3478,.T.);
#4674=ORIENTED_EDGE('',*,*,#3479,.T.);
#4675=ORIENTED_EDGE('',*,*,#3480,.T.);
#4676=ORIENTED_EDGE('',*,*,#3474,.T.);
#4677=ORIENTED_EDGE('',*,*,#3481,.T.);
#4678=ORIENTED_EDGE('',*,*,#3482,.T.);
#4679=ORIENTED_EDGE('',*,*,#3413,.F.);
#4680=ORIENTED_EDGE('',*,*,#3473,.T.);
#4681=ORIENTED_EDGE('',*,*,#3480,.F.);
#4682=ORIENTED_EDGE('',*,*,#3483,.F.);
#4683=ORIENTED_EDGE('',*,*,#3481,.F.);
#4684=ORIENTED_EDGE('',*,*,#3484,.T.);
#4685=ORIENTED_EDGE('',*,*,#3485,.T.);
#4686=ORIENTED_EDGE('',*,*,#3483,.T.);
#4687=ORIENTED_EDGE('',*,*,#3486,.T.);
#4688=ORIENTED_EDGE('',*,*,#3487,.T.);
#4689=ORIENTED_EDGE('',*,*,#3488,.T.);
#4690=ORIENTED_EDGE('',*,*,#3477,.T.);
#4691=ORIENTED_EDGE('',*,*,#3489,.T.);
#4692=ORIENTED_EDGE('',*,*,#3490,.T.);
#4693=ORIENTED_EDGE('',*,*,#3484,.F.);
#4694=ORIENTED_EDGE('',*,*,#3479,.F.);
#4695=ORIENTED_EDGE('',*,*,#3490,.F.);
#4696=ORIENTED_EDGE('',*,*,#3403,.F.);
#4697=ORIENTED_EDGE('',*,*,#3424,.F.);
#4698=ORIENTED_EDGE('',*,*,#3404,.F.);
#4699=ORIENTED_EDGE('',*,*,#3489,.F.);
#4700=ORIENTED_EDGE('',*,*,#3475,.F.);
#4701=ORIENTED_EDGE('',*,*,#3491,.T.);
#4702=ORIENTED_EDGE('',*,*,#3449,.T.);
#4703=ORIENTED_EDGE('',*,*,#3492,.T.);
#4704=ORIENTED_EDGE('',*,*,#3492,.F.);
#4705=ORIENTED_EDGE('',*,*,#3451,.F.);
#4706=ORIENTED_EDGE('',*,*,#3488,.F.);
#4707=ORIENTED_EDGE('',*,*,#3493,.F.);
#4708=ORIENTED_EDGE('',*,*,#3432,.F.);
#4709=ORIENTED_EDGE('',*,*,#3447,.F.);
#4710=ORIENTED_EDGE('',*,*,#3491,.F.);
#4711=ORIENTED_EDGE('',*,*,#3494,.F.);
#4712=ORIENTED_EDGE('',*,*,#3434,.F.);
#4713=ORIENTED_EDGE('',*,*,#3495,.F.);
#4714=ORIENTED_EDGE('',*,*,#3487,.F.);
#4715=ORIENTED_EDGE('',*,*,#3452,.F.);
#4716=ORIENTED_EDGE('',*,*,#3442,.T.);
#4717=ORIENTED_EDGE('',*,*,#3453,.F.);
#4718=ORIENTED_EDGE('',*,*,#3486,.F.);
#4719=ORIENTED_EDGE('',*,*,#3450,.F.);
#4720=ORIENTED_EDGE('',*,*,#3414,.F.);
#4721=ORIENTED_EDGE('',*,*,#3482,.F.);
#4722=ORIENTED_EDGE('',*,*,#3485,.F.);
#4723=ORIENTED_EDGE('',*,*,#3402,.F.);
#4724=ORIENTED_EDGE('',*,*,#3494,.T.);
#4725=ORIENTED_EDGE('',*,*,#3493,.T.);
#4726=ORIENTED_EDGE('',*,*,#3495,.T.);
#4727=ORIENTED_EDGE('',*,*,#3433,.F.);
#4728=ORIENTED_EDGE('',*,*,#3496,.F.);
#4729=ORIENTED_EDGE('',*,*,#3497,.F.);
#4730=ORIENTED_EDGE('',*,*,#3498,.F.);
#4731=ORIENTED_EDGE('',*,*,#3499,.F.);
#4732=ORIENTED_EDGE('',*,*,#3500,.F.);
#4733=ORIENTED_EDGE('',*,*,#3501,.F.);
#4734=ORIENTED_EDGE('',*,*,#3502,.F.);
#4735=ORIENTED_EDGE('',*,*,#3503,.F.);
#4736=ORIENTED_EDGE('',*,*,#3504,.F.);
#4737=ORIENTED_EDGE('',*,*,#3496,.T.);
#4738=ORIENTED_EDGE('',*,*,#3505,.T.);
#4739=ORIENTED_EDGE('',*,*,#3503,.T.);
#4740=ORIENTED_EDGE('',*,*,#3506,.T.);
#4741=ORIENTED_EDGE('',*,*,#3422,.T.);
#4742=ORIENTED_EDGE('',*,*,#3507,.T.);
#4743=ORIENTED_EDGE('',*,*,#3504,.T.);
#4744=ORIENTED_EDGE('',*,*,#3508,.T.);
#4745=ORIENTED_EDGE('',*,*,#3509,.F.);
#4746=ORIENTED_EDGE('',*,*,#3510,.F.);
#4747=ORIENTED_EDGE('',*,*,#3511,.F.);
#4748=ORIENTED_EDGE('',*,*,#3510,.T.);
#4749=ORIENTED_EDGE('',*,*,#3512,.T.);
#4750=ORIENTED_EDGE('',*,*,#3500,.T.);
#4751=ORIENTED_EDGE('',*,*,#3513,.T.);
#4752=ORIENTED_EDGE('',*,*,#3502,.T.);
#4753=ORIENTED_EDGE('',*,*,#3514,.T.);
#4754=ORIENTED_EDGE('',*,*,#3511,.T.);
#4755=ORIENTED_EDGE('',*,*,#3515,.T.);
#4756=ORIENTED_EDGE('',*,*,#3420,.T.);
#4757=ORIENTED_EDGE('',*,*,#3516,.T.);
#4758=ORIENTED_EDGE('',*,*,#3509,.T.);
#4759=ORIENTED_EDGE('',*,*,#3517,.T.);
#4760=ORIENTED_EDGE('',*,*,#3418,.T.);
#4761=ORIENTED_EDGE('',*,*,#3518,.T.);
#4762=ORIENTED_EDGE('',*,*,#3501,.T.);
#4763=ORIENTED_EDGE('',*,*,#3519,.T.);
#4764=ORIENTED_EDGE('',*,*,#3499,.T.);
#4765=ORIENTED_EDGE('',*,*,#3520,.T.);
#4766=ORIENTED_EDGE('',*,*,#3497,.T.);
#4767=ORIENTED_EDGE('',*,*,#3521,.T.);
#4768=ORIENTED_EDGE('',*,*,#3416,.T.);
#4769=ORIENTED_EDGE('',*,*,#3522,.T.);
#4770=ORIENTED_EDGE('',*,*,#3498,.T.);
#4771=ORIENTED_EDGE('',*,*,#3523,.T.);
#4772=ORIENTED_EDGE('',*,*,#3517,.F.);
#4773=ORIENTED_EDGE('',*,*,#3514,.F.);
#4774=ORIENTED_EDGE('',*,*,#3507,.F.);
#4775=ORIENTED_EDGE('',*,*,#3421,.F.);
#4776=ORIENTED_EDGE('',*,*,#3339,.T.);
#4777=ORIENTED_EDGE('',*,*,#3423,.F.);
#4778=ORIENTED_EDGE('',*,*,#3508,.F.);
#4779=ORIENTED_EDGE('',*,*,#3505,.F.);
#4780=ORIENTED_EDGE('',*,*,#3522,.F.);
#4781=ORIENTED_EDGE('',*,*,#3415,.F.);
#4782=ORIENTED_EDGE('',*,*,#3355,.T.);
#4783=ORIENTED_EDGE('',*,*,#3368,.T.);
#4784=ORIENTED_EDGE('',*,*,#3513,.F.);
#4785=ORIENTED_EDGE('',*,*,#3521,.F.);
#4786=ORIENTED_EDGE('',*,*,#3506,.F.);
#4787=ORIENTED_EDGE('',*,*,#3515,.F.);
#4788=ORIENTED_EDGE('',*,*,#3329,.T.);
#4789=ORIENTED_EDGE('',*,*,#3325,.T.);
#4790=ORIENTED_EDGE('',*,*,#3323,.T.);
#4791=ORIENTED_EDGE('',*,*,#3320,.T.);
#4792=ORIENTED_EDGE('',*,*,#3317,.T.);
#4793=ORIENTED_EDGE('',*,*,#3315,.T.);
#4794=ORIENTED_EDGE('',*,*,#3518,.F.);
#4795=ORIENTED_EDGE('',*,*,#3417,.F.);
#4796=ORIENTED_EDGE('',*,*,#3523,.F.);
#4797=ORIENTED_EDGE('',*,*,#3520,.F.);
#4798=ORIENTED_EDGE('',*,*,#3516,.F.);
#4799=ORIENTED_EDGE('',*,*,#3419,.F.);
#4800=ORIENTED_EDGE('',*,*,#3519,.F.);
#4801=ORIENTED_EDGE('',*,*,#3512,.F.);
#4802=ORIENTED_EDGE('',*,*,#3524,.F.);
#4803=ORIENTED_EDGE('',*,*,#3525,.T.);
#4804=ORIENTED_EDGE('',*,*,#3526,.F.);
#4805=ORIENTED_EDGE('',*,*,#3527,.T.);
#4806=ORIENTED_EDGE('',*,*,#3528,.F.);
#4807=ORIENTED_EDGE('',*,*,#3529,.T.);
#4808=ORIENTED_EDGE('',*,*,#3530,.F.);
#4809=ORIENTED_EDGE('',*,*,#3531,.T.);
#4810=ORIENTED_EDGE('',*,*,#3526,.T.);
#4811=ORIENTED_EDGE('',*,*,#3532,.F.);
#4812=ORIENTED_EDGE('',*,*,#3533,.T.);
#4813=ORIENTED_EDGE('',*,*,#3534,.F.);
#4814=ORIENTED_EDGE('',*,*,#3535,.T.);
#4815=ORIENTED_EDGE('',*,*,#3536,.F.);
#4816=ORIENTED_EDGE('',*,*,#3530,.T.);
#4817=ORIENTED_EDGE('',*,*,#3537,.F.);
#4818=ORIENTED_EDGE('',*,*,#3538,.T.);
#4819=ORIENTED_EDGE('',*,*,#3539,.F.);
#4820=ORIENTED_EDGE('',*,*,#3540,.T.);
#4821=ORIENTED_EDGE('',*,*,#3541,.F.);
#4822=ORIENTED_EDGE('',*,*,#3542,.T.);
#4823=ORIENTED_EDGE('',*,*,#3543,.T.);
#4824=ORIENTED_EDGE('',*,*,#3537,.T.);
#4825=ORIENTED_EDGE('',*,*,#3531,.F.);
#4826=ORIENTED_EDGE('',*,*,#3541,.T.);
#4827=ORIENTED_EDGE('',*,*,#3544,.T.);
#4828=ORIENTED_EDGE('',*,*,#3545,.T.);
#4829=ORIENTED_EDGE('',*,*,#3525,.F.);
#4830=ORIENTED_EDGE('',*,*,#3546,.T.);
#4831=ORIENTED_EDGE('',*,*,#3547,.T.);
#4832=ORIENTED_EDGE('',*,*,#3548,.T.);
#4833=ORIENTED_EDGE('',*,*,#3549,.F.);
#4834=ORIENTED_EDGE('',*,*,#3550,.T.);
#4835=ORIENTED_EDGE('',*,*,#3551,.T.);
#4836=ORIENTED_EDGE('',*,*,#3552,.F.);
#4837=ORIENTED_EDGE('',*,*,#3553,.F.);
#4838=ORIENTED_EDGE('',*,*,#3554,.T.);
#4839=ORIENTED_EDGE('',*,*,#3555,.T.);
#4840=ORIENTED_EDGE('',*,*,#3550,.F.);
#4841=ORIENTED_EDGE('',*,*,#3556,.F.);
#4842=ORIENTED_EDGE('',*,*,#3557,.T.);
#4843=ORIENTED_EDGE('',*,*,#3558,.T.);
#4844=ORIENTED_EDGE('',*,*,#3554,.F.);
#4845=ORIENTED_EDGE('',*,*,#3559,.F.);
#4846=ORIENTED_EDGE('',*,*,#3560,.T.);
#4847=ORIENTED_EDGE('',*,*,#3561,.T.);
#4848=ORIENTED_EDGE('',*,*,#3557,.F.);
#4849=ORIENTED_EDGE('',*,*,#3562,.F.);
#4850=ORIENTED_EDGE('',*,*,#3563,.T.);
#4851=ORIENTED_EDGE('',*,*,#3564,.T.);
#4852=ORIENTED_EDGE('',*,*,#3560,.F.);
#4853=ORIENTED_EDGE('',*,*,#3565,.F.);
#4854=ORIENTED_EDGE('',*,*,#3552,.T.);
#4855=ORIENTED_EDGE('',*,*,#3566,.T.);
#4856=ORIENTED_EDGE('',*,*,#3563,.F.);
#4857=ORIENTED_EDGE('',*,*,#3566,.F.);
#4858=ORIENTED_EDGE('',*,*,#3551,.F.);
#4859=ORIENTED_EDGE('',*,*,#3555,.F.);
#4860=ORIENTED_EDGE('',*,*,#3558,.F.);
#4861=ORIENTED_EDGE('',*,*,#3561,.F.);
#4862=ORIENTED_EDGE('',*,*,#3564,.F.);
#4863=ORIENTED_EDGE('',*,*,#3567,.F.);
#4864=ORIENTED_EDGE('',*,*,#3568,.F.);
#4865=ORIENTED_EDGE('',*,*,#3569,.T.);
#4866=ORIENTED_EDGE('',*,*,#3570,.T.);
#4867=ORIENTED_EDGE('',*,*,#3571,.F.);
#4868=ORIENTED_EDGE('',*,*,#3572,.F.);
#4869=ORIENTED_EDGE('',*,*,#3573,.T.);
#4870=ORIENTED_EDGE('',*,*,#3574,.T.);
#4871=ORIENTED_EDGE('',*,*,#3569,.F.);
#4872=ORIENTED_EDGE('',*,*,#3575,.F.);
#4873=ORIENTED_EDGE('',*,*,#3576,.T.);
#4874=ORIENTED_EDGE('',*,*,#3577,.T.);
#4875=ORIENTED_EDGE('',*,*,#3573,.F.);
#4876=ORIENTED_EDGE('',*,*,#3578,.F.);
#4877=ORIENTED_EDGE('',*,*,#3579,.T.);
#4878=ORIENTED_EDGE('',*,*,#3580,.T.);
#4879=ORIENTED_EDGE('',*,*,#3576,.F.);
#4880=ORIENTED_EDGE('',*,*,#3581,.F.);
#4881=ORIENTED_EDGE('',*,*,#3582,.T.);
#4882=ORIENTED_EDGE('',*,*,#3583,.T.);
#4883=ORIENTED_EDGE('',*,*,#3579,.F.);
#4884=ORIENTED_EDGE('',*,*,#3584,.F.);
#4885=ORIENTED_EDGE('',*,*,#3571,.T.);
#4886=ORIENTED_EDGE('',*,*,#3585,.T.);
#4887=ORIENTED_EDGE('',*,*,#3582,.F.);
#4888=ORIENTED_EDGE('',*,*,#3585,.F.);
#4889=ORIENTED_EDGE('',*,*,#3570,.F.);
#4890=ORIENTED_EDGE('',*,*,#3574,.F.);
#4891=ORIENTED_EDGE('',*,*,#3577,.F.);
#4892=ORIENTED_EDGE('',*,*,#3580,.F.);
#4893=ORIENTED_EDGE('',*,*,#3583,.F.);
#4894=ORIENTED_EDGE('',*,*,#3586,.F.);
#4895=ORIENTED_EDGE('',*,*,#3587,.F.);
#4896=ORIENTED_EDGE('',*,*,#3588,.T.);
#4897=ORIENTED_EDGE('',*,*,#3546,.F.);
#4898=ORIENTED_EDGE('',*,*,#3588,.F.);
#4899=ORIENTED_EDGE('',*,*,#3589,.F.);
#4900=ORIENTED_EDGE('',*,*,#3590,.T.);
#4901=ORIENTED_EDGE('',*,*,#3591,.F.);
#4902=ORIENTED_EDGE('',*,*,#3590,.F.);
#4903=ORIENTED_EDGE('',*,*,#3592,.F.);
#4904=ORIENTED_EDGE('',*,*,#3593,.T.);
#4905=ORIENTED_EDGE('',*,*,#3594,.F.);
#4906=ORIENTED_EDGE('',*,*,#3593,.F.);
#4907=ORIENTED_EDGE('',*,*,#3595,.F.);
#4908=ORIENTED_EDGE('',*,*,#3596,.T.);
#4909=ORIENTED_EDGE('',*,*,#3547,.F.);
#4910=ORIENTED_EDGE('',*,*,#3596,.F.);
#4911=ORIENTED_EDGE('',*,*,#3586,.T.);
#4912=ORIENTED_EDGE('',*,*,#3597,.T.);
#4913=ORIENTED_EDGE('',*,*,#3598,.F.);
#4914=ORIENTED_EDGE('',*,*,#3597,.F.);
#4915=ORIENTED_EDGE('',*,*,#3567,.T.);
#4916=ORIENTED_EDGE('',*,*,#3599,.T.);
#4917=ORIENTED_EDGE('',*,*,#3600,.F.);
#4918=ORIENTED_EDGE('',*,*,#3599,.F.);
#4919=ORIENTED_EDGE('',*,*,#3601,.F.);
#4920=ORIENTED_EDGE('',*,*,#3602,.F.);
#4921=ORIENTED_EDGE('',*,*,#3603,.F.);
#4922=ORIENTED_EDGE('',*,*,#3604,.T.);
#4923=ORIENTED_EDGE('',*,*,#3605,.F.);
#4924=ORIENTED_EDGE('',*,*,#3606,.T.);
#4925=ORIENTED_EDGE('',*,*,#3607,.F.);
#4926=ORIENTED_EDGE('',*,*,#3608,.F.);
#4927=ORIENTED_EDGE('',*,*,#3609,.F.);
#4928=ORIENTED_EDGE('',*,*,#3610,.T.);
#4929=ORIENTED_EDGE('',*,*,#3611,.F.);
#4930=ORIENTED_EDGE('',*,*,#3612,.F.);
#4931=ORIENTED_EDGE('',*,*,#3613,.F.);
#4932=ORIENTED_EDGE('',*,*,#3614,.T.);
#4933=ORIENTED_EDGE('',*,*,#3615,.F.);
#4934=ORIENTED_EDGE('',*,*,#3616,.F.);
#4935=ORIENTED_EDGE('',*,*,#3617,.F.);
#4936=ORIENTED_EDGE('',*,*,#3618,.T.);
#4937=ORIENTED_EDGE('',*,*,#3619,.F.);
#4938=ORIENTED_EDGE('',*,*,#3620,.F.);
#4939=ORIENTED_EDGE('',*,*,#3621,.F.);
#4940=ORIENTED_EDGE('',*,*,#3622,.F.);
#4941=ORIENTED_EDGE('',*,*,#3623,.F.);
#4942=ORIENTED_EDGE('',*,*,#3624,.T.);
#4943=ORIENTED_EDGE('',*,*,#3625,.F.);
#4944=ORIENTED_EDGE('',*,*,#3626,.F.);
#4945=ORIENTED_EDGE('',*,*,#3627,.F.);
#4946=ORIENTED_EDGE('',*,*,#3628,.T.);
#4947=ORIENTED_EDGE('',*,*,#3629,.F.);
#4948=ORIENTED_EDGE('',*,*,#3598,.T.);
#4949=ORIENTED_EDGE('',*,*,#3630,.F.);
#4950=ORIENTED_EDGE('',*,*,#3600,.T.);
#4951=ORIENTED_EDGE('',*,*,#3631,.F.);
#4952=ORIENTED_EDGE('',*,*,#3604,.F.);
#4953=ORIENTED_EDGE('',*,*,#3632,.F.);
#4954=ORIENTED_EDGE('',*,*,#3618,.F.);
#4955=ORIENTED_EDGE('',*,*,#3633,.F.);
#4956=ORIENTED_EDGE('',*,*,#3624,.F.);
#4957=ORIENTED_EDGE('',*,*,#3634,.F.);
#4958=ORIENTED_EDGE('',*,*,#3606,.F.);
#4959=ORIENTED_EDGE('',*,*,#3635,.F.);
#4960=ORIENTED_EDGE('',*,*,#3628,.F.);
#4961=ORIENTED_EDGE('',*,*,#3636,.F.);
#4962=ORIENTED_EDGE('',*,*,#3610,.F.);
#4963=ORIENTED_EDGE('',*,*,#3637,.F.);
#4964=ORIENTED_EDGE('',*,*,#3638,.F.);
#4965=ORIENTED_EDGE('',*,*,#3639,.F.);
#4966=ORIENTED_EDGE('',*,*,#3614,.F.);
#4967=ORIENTED_EDGE('',*,*,#3640,.F.);
#4968=ORIENTED_EDGE('',*,*,#3641,.F.);
#4969=ORIENTED_EDGE('',*,*,#3642,.F.);
#4970=ORIENTED_EDGE('',*,*,#3638,.T.);
#4971=ORIENTED_EDGE('',*,*,#3643,.T.);
#4972=ORIENTED_EDGE('',*,*,#3644,.F.);
#4973=ORIENTED_EDGE('',*,*,#3645,.F.);
#4974=ORIENTED_EDGE('',*,*,#3544,.F.);
#4975=ORIENTED_EDGE('',*,*,#3540,.F.);
#4976=ORIENTED_EDGE('',*,*,#3646,.F.);
#4977=ORIENTED_EDGE('',*,*,#3615,.T.);
#4978=ORIENTED_EDGE('',*,*,#3639,.T.);
#4979=ORIENTED_EDGE('',*,*,#3642,.T.);
#4980=ORIENTED_EDGE('',*,*,#3647,.T.);
#4981=ORIENTED_EDGE('',*,*,#3648,.F.);
#4982=ORIENTED_EDGE('',*,*,#3538,.F.);
#4983=ORIENTED_EDGE('',*,*,#3543,.F.);
#4984=ORIENTED_EDGE('',*,*,#3649,.F.);
#4985=ORIENTED_EDGE('',*,*,#3650,.F.);
#4986=ORIENTED_EDGE('',*,*,#3651,.T.);
#4987=ORIENTED_EDGE('',*,*,#3611,.T.);
#4988=ORIENTED_EDGE('',*,*,#3636,.T.);
#4989=ORIENTED_EDGE('',*,*,#3627,.T.);
#4990=ORIENTED_EDGE('',*,*,#3652,.T.);
#4991=ORIENTED_EDGE('',*,*,#3653,.F.);
#4992=ORIENTED_EDGE('',*,*,#3654,.F.);
#4993=ORIENTED_EDGE('',*,*,#3655,.F.);
#4994=ORIENTED_EDGE('',*,*,#3656,.F.);
#4995=ORIENTED_EDGE('',*,*,#3657,.F.);
#4996=ORIENTED_EDGE('',*,*,#3658,.T.);
#4997=ORIENTED_EDGE('',*,*,#3607,.T.);
#4998=ORIENTED_EDGE('',*,*,#3634,.T.);
#4999=ORIENTED_EDGE('',*,*,#3623,.T.);
#5000=ORIENTED_EDGE('',*,*,#3659,.T.);
#5001=ORIENTED_EDGE('',*,*,#3660,.F.);
#5002=ORIENTED_EDGE('',*,*,#3533,.F.);
#5003=ORIENTED_EDGE('',*,*,#3661,.F.);
#5004=ORIENTED_EDGE('',*,*,#3662,.F.);
#5005=ORIENTED_EDGE('',*,*,#3663,.F.);
#5006=ORIENTED_EDGE('',*,*,#3664,.T.);
#5007=ORIENTED_EDGE('',*,*,#3601,.T.);
#5008=ORIENTED_EDGE('',*,*,#3631,.T.);
#5009=ORIENTED_EDGE('',*,*,#3617,.T.);
#5010=ORIENTED_EDGE('',*,*,#3665,.F.);
#5011=ORIENTED_EDGE('',*,*,#3666,.T.);
#5012=ORIENTED_EDGE('',*,*,#3667,.T.);
#5013=ORIENTED_EDGE('',*,*,#3668,.T.);
#5014=ORIENTED_EDGE('',*,*,#3669,.F.);
#5015=ORIENTED_EDGE('',*,*,#3616,.T.);
#5016=ORIENTED_EDGE('',*,*,#3651,.F.);
#5017=ORIENTED_EDGE('',*,*,#3670,.T.);
#5018=ORIENTED_EDGE('',*,*,#3643,.F.);
#5019=ORIENTED_EDGE('',*,*,#3671,.T.);
#5020=ORIENTED_EDGE('',*,*,#3647,.F.);
#5021=ORIENTED_EDGE('',*,*,#3641,.T.);
#5022=ORIENTED_EDGE('',*,*,#3672,.F.);
#5023=ORIENTED_EDGE('',*,*,#3673,.T.);
#5024=ORIENTED_EDGE('',*,*,#3652,.F.);
#5025=ORIENTED_EDGE('',*,*,#3626,.T.);
#5026=ORIENTED_EDGE('',*,*,#3674,.F.);
#5027=ORIENTED_EDGE('',*,*,#3675,.T.);
#5028=ORIENTED_EDGE('',*,*,#3659,.F.);
#5029=ORIENTED_EDGE('',*,*,#3622,.T.);
#5030=ORIENTED_EDGE('',*,*,#3676,.F.);
#5031=ORIENTED_EDGE('',*,*,#3677,.T.);
#5032=ORIENTED_EDGE('',*,*,#3678,.T.);
#5033=ORIENTED_EDGE('',*,*,#3665,.T.);
#5034=ORIENTED_EDGE('',*,*,#3620,.T.);
#5035=ORIENTED_EDGE('',*,*,#3679,.T.);
#5036=ORIENTED_EDGE('',*,*,#3680,.F.);
#5037=ORIENTED_EDGE('',*,*,#3681,.T.);
#5038=ORIENTED_EDGE('',*,*,#3682,.F.);
#5039=ORIENTED_EDGE('',*,*,#3683,.T.);
#5040=ORIENTED_EDGE('',*,*,#3684,.F.);
#5041=ORIENTED_EDGE('',*,*,#3685,.T.);
#5042=ORIENTED_EDGE('',*,*,#3686,.F.);
#5043=ORIENTED_EDGE('',*,*,#3687,.T.);
#5044=ORIENTED_EDGE('',*,*,#3602,.T.);
#5045=ORIENTED_EDGE('',*,*,#3669,.T.);
#5046=ORIENTED_EDGE('',*,*,#3688,.T.);
#5047=ORIENTED_EDGE('',*,*,#3689,.T.);
#5048=ORIENTED_EDGE('',*,*,#3690,.F.);
#5049=ORIENTED_EDGE('',*,*,#3608,.T.);
#5050=ORIENTED_EDGE('',*,*,#3664,.F.);
#5051=ORIENTED_EDGE('',*,*,#3691,.T.);
#5052=ORIENTED_EDGE('',*,*,#3692,.F.);
#5053=ORIENTED_EDGE('',*,*,#3612,.T.);
#5054=ORIENTED_EDGE('',*,*,#3658,.F.);
#5055=ORIENTED_EDGE('',*,*,#3693,.T.);
#5056=ORIENTED_EDGE('',*,*,#3694,.F.);
#5057=ORIENTED_EDGE('',*,*,#3695,.T.);
#5058=ORIENTED_EDGE('',*,*,#3696,.T.);
#5059=ORIENTED_EDGE('',*,*,#3697,.T.);
#5060=ORIENTED_EDGE('',*,*,#3698,.T.);
#5061=ORIENTED_EDGE('',*,*,#3699,.T.);
#5062=ORIENTED_EDGE('',*,*,#3700,.F.);
#5063=ORIENTED_EDGE('',*,*,#3548,.F.);
#5064=ORIENTED_EDGE('',*,*,#3701,.T.);
#5065=ORIENTED_EDGE('',*,*,#3630,.T.);
#5066=ORIENTED_EDGE('',*,*,#3701,.F.);
#5067=ORIENTED_EDGE('',*,*,#3702,.F.);
#5068=ORIENTED_EDGE('',*,*,#3703,.T.);
#5069=ORIENTED_EDGE('',*,*,#3629,.T.);
#5070=ORIENTED_EDGE('',*,*,#3703,.F.);
#5071=ORIENTED_EDGE('',*,*,#3704,.F.);
#5072=ORIENTED_EDGE('',*,*,#3700,.T.);
#5073=ORIENTED_EDGE('',*,*,#3705,.F.);
#5074=ORIENTED_EDGE('',*,*,#3706,.F.);
#5075=ORIENTED_EDGE('',*,*,#3707,.F.);
#5076=ORIENTED_EDGE('',*,*,#3708,.F.);
#5077=ORIENTED_EDGE('',*,*,#3644,.T.);
#5078=ORIENTED_EDGE('',*,*,#3670,.F.);
#5079=ORIENTED_EDGE('',*,*,#3650,.T.);
#5080=ORIENTED_EDGE('',*,*,#3709,.T.);
#5081=ORIENTED_EDGE('',*,*,#3704,.T.);
#5082=ORIENTED_EDGE('',*,*,#3710,.T.);
#5083=ORIENTED_EDGE('',*,*,#3711,.T.);
#5084=ORIENTED_EDGE('',*,*,#3695,.F.);
#5085=ORIENTED_EDGE('',*,*,#3524,.T.);
#5086=ORIENTED_EDGE('',*,*,#3545,.F.);
#5087=ORIENTED_EDGE('',*,*,#3645,.T.);
#5088=ORIENTED_EDGE('',*,*,#3709,.F.);
#5089=ORIENTED_EDGE('',*,*,#3649,.T.);
#5090=ORIENTED_EDGE('',*,*,#3542,.F.);
#5091=ORIENTED_EDGE('',*,*,#3708,.T.);
#5092=ORIENTED_EDGE('',*,*,#3712,.F.);
#5093=ORIENTED_EDGE('',*,*,#3713,.F.);
#5094=ORIENTED_EDGE('',*,*,#3710,.F.);
#5095=ORIENTED_EDGE('',*,*,#3707,.T.);
#5096=ORIENTED_EDGE('',*,*,#3714,.T.);
#5097=ORIENTED_EDGE('',*,*,#3715,.T.);
#5098=ORIENTED_EDGE('',*,*,#3712,.T.);
#5099=ORIENTED_EDGE('',*,*,#3646,.T.);
#5100=ORIENTED_EDGE('',*,*,#3539,.T.);
#5101=ORIENTED_EDGE('',*,*,#3648,.T.);
#5102=ORIENTED_EDGE('',*,*,#3671,.F.);
#5103=ORIENTED_EDGE('',*,*,#3705,.T.);
#5104=ORIENTED_EDGE('',*,*,#3699,.F.);
#5105=ORIENTED_EDGE('',*,*,#3716,.T.);
#5106=ORIENTED_EDGE('',*,*,#3717,.T.);
#5107=ORIENTED_EDGE('',*,*,#3613,.T.);
#5108=ORIENTED_EDGE('',*,*,#3694,.T.);
#5109=ORIENTED_EDGE('',*,*,#3718,.F.);
#5110=ORIENTED_EDGE('',*,*,#3719,.F.);
#5111=ORIENTED_EDGE('',*,*,#3720,.F.);
#5112=ORIENTED_EDGE('',*,*,#3721,.F.);
#5113=ORIENTED_EDGE('',*,*,#3722,.F.);
#5114=ORIENTED_EDGE('',*,*,#3672,.T.);
#5115=ORIENTED_EDGE('',*,*,#3640,.T.);
#5116=ORIENTED_EDGE('',*,*,#3637,.T.);
#5117=ORIENTED_EDGE('',*,*,#3718,.T.);
#5118=ORIENTED_EDGE('',*,*,#3693,.F.);
#5119=ORIENTED_EDGE('',*,*,#3657,.T.);
#5120=ORIENTED_EDGE('',*,*,#3723,.T.);
#5121=ORIENTED_EDGE('',*,*,#3719,.T.);
#5122=ORIENTED_EDGE('',*,*,#3723,.F.);
#5123=ORIENTED_EDGE('',*,*,#3656,.T.);
#5124=ORIENTED_EDGE('',*,*,#3724,.F.);
#5125=ORIENTED_EDGE('',*,*,#3720,.T.);
#5126=ORIENTED_EDGE('',*,*,#3724,.T.);
#5127=ORIENTED_EDGE('',*,*,#3655,.T.);
#5128=ORIENTED_EDGE('',*,*,#3725,.T.);
#5129=ORIENTED_EDGE('',*,*,#3721,.T.);
#5130=ORIENTED_EDGE('',*,*,#3725,.F.);
#5131=ORIENTED_EDGE('',*,*,#3654,.T.);
#5132=ORIENTED_EDGE('',*,*,#3726,.F.);
#5133=ORIENTED_EDGE('',*,*,#3722,.T.);
#5134=ORIENTED_EDGE('',*,*,#3726,.T.);
#5135=ORIENTED_EDGE('',*,*,#3653,.T.);
#5136=ORIENTED_EDGE('',*,*,#3673,.F.);
#5137=ORIENTED_EDGE('',*,*,#3609,.T.);
#5138=ORIENTED_EDGE('',*,*,#3692,.T.);
#5139=ORIENTED_EDGE('',*,*,#3727,.F.);
#5140=ORIENTED_EDGE('',*,*,#3728,.F.);
#5141=ORIENTED_EDGE('',*,*,#3729,.F.);
#5142=ORIENTED_EDGE('',*,*,#3535,.F.);
#5143=ORIENTED_EDGE('',*,*,#3730,.F.);
#5144=ORIENTED_EDGE('',*,*,#3674,.T.);
#5145=ORIENTED_EDGE('',*,*,#3625,.T.);
#5146=ORIENTED_EDGE('',*,*,#3635,.T.);
#5147=ORIENTED_EDGE('',*,*,#3727,.T.);
#5148=ORIENTED_EDGE('',*,*,#3691,.F.);
#5149=ORIENTED_EDGE('',*,*,#3663,.T.);
#5150=ORIENTED_EDGE('',*,*,#3731,.T.);
#5151=ORIENTED_EDGE('',*,*,#3528,.T.);
#5152=ORIENTED_EDGE('',*,*,#3732,.F.);
#5153=ORIENTED_EDGE('',*,*,#3728,.T.);
#5154=ORIENTED_EDGE('',*,*,#3731,.F.);
#5155=ORIENTED_EDGE('',*,*,#3662,.T.);
#5156=ORIENTED_EDGE('',*,*,#3733,.F.);
#5157=ORIENTED_EDGE('',*,*,#3536,.T.);
#5158=ORIENTED_EDGE('',*,*,#3729,.T.);
#5159=ORIENTED_EDGE('',*,*,#3732,.T.);
#5160=ORIENTED_EDGE('',*,*,#3529,.F.);
#5161=ORIENTED_EDGE('',*,*,#3733,.T.);
#5162=ORIENTED_EDGE('',*,*,#3661,.T.);
#5163=ORIENTED_EDGE('',*,*,#3532,.T.);
#5164=ORIENTED_EDGE('',*,*,#3527,.F.);
#5165=ORIENTED_EDGE('',*,*,#3594,.T.);
#5166=ORIENTED_EDGE('',*,*,#3591,.T.);
#5167=ORIENTED_EDGE('',*,*,#3702,.T.);
#5168=ORIENTED_EDGE('',*,*,#3730,.T.);
#5169=ORIENTED_EDGE('',*,*,#3534,.T.);
#5170=ORIENTED_EDGE('',*,*,#3660,.T.);
#5171=ORIENTED_EDGE('',*,*,#3675,.F.);
#5172=ORIENTED_EDGE('',*,*,#3605,.T.);
#5173=ORIENTED_EDGE('',*,*,#3690,.T.);
#5174=ORIENTED_EDGE('',*,*,#3734,.F.);
#5175=ORIENTED_EDGE('',*,*,#3735,.F.);
#5176=ORIENTED_EDGE('',*,*,#3736,.F.);
#5177=ORIENTED_EDGE('',*,*,#3737,.F.);
#5178=ORIENTED_EDGE('',*,*,#3738,.F.);
#5179=ORIENTED_EDGE('',*,*,#3676,.T.);
#5180=ORIENTED_EDGE('',*,*,#3621,.T.);
#5181=ORIENTED_EDGE('',*,*,#3633,.T.);
#5182=ORIENTED_EDGE('',*,*,#3734,.T.);
#5183=ORIENTED_EDGE('',*,*,#3689,.F.);
#5184=ORIENTED_EDGE('',*,*,#3739,.T.);
#5185=ORIENTED_EDGE('',*,*,#3740,.T.);
#5186=ORIENTED_EDGE('',*,*,#3735,.T.);
#5187=ORIENTED_EDGE('',*,*,#3740,.F.);
#5188=ORIENTED_EDGE('',*,*,#3741,.F.);
#5189=ORIENTED_EDGE('',*,*,#3742,.F.);
#5190=ORIENTED_EDGE('',*,*,#3736,.T.);
#5191=ORIENTED_EDGE('',*,*,#3742,.T.);
#5192=ORIENTED_EDGE('',*,*,#3743,.T.);
#5193=ORIENTED_EDGE('',*,*,#3744,.T.);
#5194=ORIENTED_EDGE('',*,*,#3738,.T.);
#5195=ORIENTED_EDGE('',*,*,#3745,.T.);
#5196=ORIENTED_EDGE('',*,*,#3746,.T.);
#5197=ORIENTED_EDGE('',*,*,#3677,.F.);
#5198=ORIENTED_EDGE('',*,*,#3737,.T.);
#5199=ORIENTED_EDGE('',*,*,#3744,.F.);
#5200=ORIENTED_EDGE('',*,*,#3747,.F.);
#5201=ORIENTED_EDGE('',*,*,#3745,.F.);
#5202=ORIENTED_EDGE('',*,*,#3748,.T.);
#5203=ORIENTED_EDGE('',*,*,#3749,.T.);
#5204=ORIENTED_EDGE('',*,*,#3747,.T.);
#5205=ORIENTED_EDGE('',*,*,#3750,.T.);
#5206=ORIENTED_EDGE('',*,*,#3751,.T.);
#5207=ORIENTED_EDGE('',*,*,#3752,.T.);
#5208=ORIENTED_EDGE('',*,*,#3741,.T.);
#5209=ORIENTED_EDGE('',*,*,#3753,.T.);
#5210=ORIENTED_EDGE('',*,*,#3754,.T.);
#5211=ORIENTED_EDGE('',*,*,#3748,.F.);
#5212=ORIENTED_EDGE('',*,*,#3743,.F.);
#5213=ORIENTED_EDGE('',*,*,#3754,.F.);
#5214=ORIENTED_EDGE('',*,*,#3667,.F.);
#5215=ORIENTED_EDGE('',*,*,#3688,.F.);
#5216=ORIENTED_EDGE('',*,*,#3668,.F.);
#5217=ORIENTED_EDGE('',*,*,#3753,.F.);
#5218=ORIENTED_EDGE('',*,*,#3739,.F.);
#5219=ORIENTED_EDGE('',*,*,#3755,.T.);
#5220=ORIENTED_EDGE('',*,*,#3713,.T.);
#5221=ORIENTED_EDGE('',*,*,#3756,.T.);
#5222=ORIENTED_EDGE('',*,*,#3756,.F.);
#5223=ORIENTED_EDGE('',*,*,#3715,.F.);
#5224=ORIENTED_EDGE('',*,*,#3752,.F.);
#5225=ORIENTED_EDGE('',*,*,#3757,.F.);
#5226=ORIENTED_EDGE('',*,*,#3696,.F.);
#5227=ORIENTED_EDGE('',*,*,#3711,.F.);
#5228=ORIENTED_EDGE('',*,*,#3755,.F.);
#5229=ORIENTED_EDGE('',*,*,#3758,.F.);
#5230=ORIENTED_EDGE('',*,*,#3698,.F.);
#5231=ORIENTED_EDGE('',*,*,#3759,.F.);
#5232=ORIENTED_EDGE('',*,*,#3751,.F.);
#5233=ORIENTED_EDGE('',*,*,#3716,.F.);
#5234=ORIENTED_EDGE('',*,*,#3706,.T.);
#5235=ORIENTED_EDGE('',*,*,#3717,.F.);
#5236=ORIENTED_EDGE('',*,*,#3750,.F.);
#5237=ORIENTED_EDGE('',*,*,#3714,.F.);
#5238=ORIENTED_EDGE('',*,*,#3678,.F.);
#5239=ORIENTED_EDGE('',*,*,#3746,.F.);
#5240=ORIENTED_EDGE('',*,*,#3749,.F.);
#5241=ORIENTED_EDGE('',*,*,#3666,.F.);
#5242=ORIENTED_EDGE('',*,*,#3758,.T.);
#5243=ORIENTED_EDGE('',*,*,#3757,.T.);
#5244=ORIENTED_EDGE('',*,*,#3759,.T.);
#5245=ORIENTED_EDGE('',*,*,#3697,.F.);
#5246=ORIENTED_EDGE('',*,*,#3760,.F.);
#5247=ORIENTED_EDGE('',*,*,#3761,.F.);
#5248=ORIENTED_EDGE('',*,*,#3762,.F.);
#5249=ORIENTED_EDGE('',*,*,#3763,.F.);
#5250=ORIENTED_EDGE('',*,*,#3764,.F.);
#5251=ORIENTED_EDGE('',*,*,#3765,.F.);
#5252=ORIENTED_EDGE('',*,*,#3766,.F.);
#5253=ORIENTED_EDGE('',*,*,#3767,.F.);
#5254=ORIENTED_EDGE('',*,*,#3768,.F.);
#5255=ORIENTED_EDGE('',*,*,#3760,.T.);
#5256=ORIENTED_EDGE('',*,*,#3769,.T.);
#5257=ORIENTED_EDGE('',*,*,#3767,.T.);
#5258=ORIENTED_EDGE('',*,*,#3770,.T.);
#5259=ORIENTED_EDGE('',*,*,#3686,.T.);
#5260=ORIENTED_EDGE('',*,*,#3771,.T.);
#5261=ORIENTED_EDGE('',*,*,#3768,.T.);
#5262=ORIENTED_EDGE('',*,*,#3772,.T.);
#5263=ORIENTED_EDGE('',*,*,#3773,.F.);
#5264=ORIENTED_EDGE('',*,*,#3774,.F.);
#5265=ORIENTED_EDGE('',*,*,#3775,.F.);
#5266=ORIENTED_EDGE('',*,*,#3774,.T.);
#5267=ORIENTED_EDGE('',*,*,#3776,.T.);
#5268=ORIENTED_EDGE('',*,*,#3764,.T.);
#5269=ORIENTED_EDGE('',*,*,#3777,.T.);
#5270=ORIENTED_EDGE('',*,*,#3766,.T.);
#5271=ORIENTED_EDGE('',*,*,#3778,.T.);
#5272=ORIENTED_EDGE('',*,*,#3775,.T.);
#5273=ORIENTED_EDGE('',*,*,#3779,.T.);
#5274=ORIENTED_EDGE('',*,*,#3684,.T.);
#5275=ORIENTED_EDGE('',*,*,#3780,.T.);
#5276=ORIENTED_EDGE('',*,*,#3773,.T.);
#5277=ORIENTED_EDGE('',*,*,#3781,.T.);
#5278=ORIENTED_EDGE('',*,*,#3682,.T.);
#5279=ORIENTED_EDGE('',*,*,#3782,.T.);
#5280=ORIENTED_EDGE('',*,*,#3765,.T.);
#5281=ORIENTED_EDGE('',*,*,#3783,.T.);
#5282=ORIENTED_EDGE('',*,*,#3763,.T.);
#5283=ORIENTED_EDGE('',*,*,#3784,.T.);
#5284=ORIENTED_EDGE('',*,*,#3761,.T.);
#5285=ORIENTED_EDGE('',*,*,#3785,.T.);
#5286=ORIENTED_EDGE('',*,*,#3680,.T.);
#5287=ORIENTED_EDGE('',*,*,#3786,.T.);
#5288=ORIENTED_EDGE('',*,*,#3762,.T.);
#5289=ORIENTED_EDGE('',*,*,#3787,.T.);
#5290=ORIENTED_EDGE('',*,*,#3781,.F.);
#5291=ORIENTED_EDGE('',*,*,#3778,.F.);
#5292=ORIENTED_EDGE('',*,*,#3771,.F.);
#5293=ORIENTED_EDGE('',*,*,#3685,.F.);
#5294=ORIENTED_EDGE('',*,*,#3603,.T.);
#5295=ORIENTED_EDGE('',*,*,#3687,.F.);
#5296=ORIENTED_EDGE('',*,*,#3772,.F.);
#5297=ORIENTED_EDGE('',*,*,#3769,.F.);
#5298=ORIENTED_EDGE('',*,*,#3786,.F.);
#5299=ORIENTED_EDGE('',*,*,#3679,.F.);
#5300=ORIENTED_EDGE('',*,*,#3619,.T.);
#5301=ORIENTED_EDGE('',*,*,#3632,.T.);
#5302=ORIENTED_EDGE('',*,*,#3777,.F.);
#5303=ORIENTED_EDGE('',*,*,#3785,.F.);
#5304=ORIENTED_EDGE('',*,*,#3770,.F.);
#5305=ORIENTED_EDGE('',*,*,#3779,.F.);
#5306=ORIENTED_EDGE('',*,*,#3549,.T.);
#5307=ORIENTED_EDGE('',*,*,#3565,.T.);
#5308=ORIENTED_EDGE('',*,*,#3562,.T.);
#5309=ORIENTED_EDGE('',*,*,#3559,.T.);
#5310=ORIENTED_EDGE('',*,*,#3556,.T.);
#5311=ORIENTED_EDGE('',*,*,#3553,.T.);
#5312=ORIENTED_EDGE('',*,*,#3568,.T.);
#5313=ORIENTED_EDGE('',*,*,#3584,.T.);
#5314=ORIENTED_EDGE('',*,*,#3581,.T.);
#5315=ORIENTED_EDGE('',*,*,#3578,.T.);
#5316=ORIENTED_EDGE('',*,*,#3575,.T.);
#5317=ORIENTED_EDGE('',*,*,#3572,.T.);
#5318=ORIENTED_EDGE('',*,*,#3595,.T.);
#5319=ORIENTED_EDGE('',*,*,#3592,.T.);
#5320=ORIENTED_EDGE('',*,*,#3589,.T.);
#5321=ORIENTED_EDGE('',*,*,#3587,.T.);
#5322=ORIENTED_EDGE('',*,*,#3782,.F.);
#5323=ORIENTED_EDGE('',*,*,#3681,.F.);
#5324=ORIENTED_EDGE('',*,*,#3787,.F.);
#5325=ORIENTED_EDGE('',*,*,#3784,.F.);
#5326=ORIENTED_EDGE('',*,*,#3780,.F.);
#5327=ORIENTED_EDGE('',*,*,#3683,.F.);
#5328=ORIENTED_EDGE('',*,*,#3783,.F.);
#5329=ORIENTED_EDGE('',*,*,#3776,.F.);
#5330=ORIENTED_EDGE('',*,*,#3788,.F.);
#5331=ORIENTED_EDGE('',*,*,#3789,.T.);
#5332=ORIENTED_EDGE('',*,*,#3790,.T.);
#5333=ORIENTED_EDGE('',*,*,#3791,.T.);
#5334=ORIENTED_EDGE('',*,*,#3792,.F.);
#5335=ORIENTED_EDGE('',*,*,#3793,.T.);
#5336=ORIENTED_EDGE('',*,*,#3788,.T.);
#5337=ORIENTED_EDGE('',*,*,#3794,.T.);
#5338=ORIENTED_EDGE('',*,*,#3795,.F.);
#5339=ORIENTED_EDGE('',*,*,#3796,.T.);
#5340=ORIENTED_EDGE('',*,*,#3792,.T.);
#5341=ORIENTED_EDGE('',*,*,#3797,.T.);
#5342=ORIENTED_EDGE('',*,*,#3798,.F.);
#5343=ORIENTED_EDGE('',*,*,#3799,.T.);
#5344=ORIENTED_EDGE('',*,*,#3795,.T.);
#5345=ORIENTED_EDGE('',*,*,#3800,.T.);
#5346=ORIENTED_EDGE('',*,*,#3801,.F.);
#5347=ORIENTED_EDGE('',*,*,#3802,.T.);
#5348=ORIENTED_EDGE('',*,*,#3798,.T.);
#5349=ORIENTED_EDGE('',*,*,#3803,.T.);
#5350=ORIENTED_EDGE('',*,*,#3804,.F.);
#5351=ORIENTED_EDGE('',*,*,#3805,.T.);
#5352=ORIENTED_EDGE('',*,*,#3801,.T.);
#5353=ORIENTED_EDGE('',*,*,#3806,.T.);
#5354=ORIENTED_EDGE('',*,*,#3807,.F.);
#5355=ORIENTED_EDGE('',*,*,#3808,.T.);
#5356=ORIENTED_EDGE('',*,*,#3804,.T.);
#5357=ORIENTED_EDGE('',*,*,#3809,.T.);
#5358=ORIENTED_EDGE('',*,*,#3810,.F.);
#5359=ORIENTED_EDGE('',*,*,#3811,.T.);
#5360=ORIENTED_EDGE('',*,*,#3807,.T.);
#5361=ORIENTED_EDGE('',*,*,#3812,.T.);
#5362=ORIENTED_EDGE('',*,*,#3813,.F.);
#5363=ORIENTED_EDGE('',*,*,#3814,.T.);
#5364=ORIENTED_EDGE('',*,*,#3810,.T.);
#5365=ORIENTED_EDGE('',*,*,#3815,.T.);
#5366=ORIENTED_EDGE('',*,*,#3816,.F.);
#5367=ORIENTED_EDGE('',*,*,#3817,.T.);
#5368=ORIENTED_EDGE('',*,*,#3813,.T.);
#5369=ORIENTED_EDGE('',*,*,#3818,.T.);
#5370=ORIENTED_EDGE('',*,*,#3819,.F.);
#5371=ORIENTED_EDGE('',*,*,#3820,.T.);
#5372=ORIENTED_EDGE('',*,*,#3816,.T.);
#5373=ORIENTED_EDGE('',*,*,#3821,.T.);
#5374=ORIENTED_EDGE('',*,*,#3822,.F.);
#5375=ORIENTED_EDGE('',*,*,#3823,.T.);
#5376=ORIENTED_EDGE('',*,*,#3819,.T.);
#5377=ORIENTED_EDGE('',*,*,#3824,.T.);
#5378=ORIENTED_EDGE('',*,*,#3825,.F.);
#5379=ORIENTED_EDGE('',*,*,#3826,.T.);
#5380=ORIENTED_EDGE('',*,*,#3822,.T.);
#5381=ORIENTED_EDGE('',*,*,#3827,.T.);
#5382=ORIENTED_EDGE('',*,*,#3828,.F.);
#5383=ORIENTED_EDGE('',*,*,#3829,.T.);
#5384=ORIENTED_EDGE('',*,*,#3825,.T.);
#5385=ORIENTED_EDGE('',*,*,#3830,.T.);
#5386=ORIENTED_EDGE('',*,*,#3831,.F.);
#5387=ORIENTED_EDGE('',*,*,#3832,.T.);
#5388=ORIENTED_EDGE('',*,*,#3828,.T.);
#5389=ORIENTED_EDGE('',*,*,#3833,.T.);
#5390=ORIENTED_EDGE('',*,*,#3834,.F.);
#5391=ORIENTED_EDGE('',*,*,#3835,.T.);
#5392=ORIENTED_EDGE('',*,*,#3831,.T.);
#5393=ORIENTED_EDGE('',*,*,#3836,.T.);
#5394=ORIENTED_EDGE('',*,*,#3837,.F.);
#5395=ORIENTED_EDGE('',*,*,#3838,.T.);
#5396=ORIENTED_EDGE('',*,*,#3834,.T.);
#5397=ORIENTED_EDGE('',*,*,#3839,.T.);
#5398=ORIENTED_EDGE('',*,*,#3840,.F.);
#5399=ORIENTED_EDGE('',*,*,#3841,.T.);
#5400=ORIENTED_EDGE('',*,*,#3837,.T.);
#5401=ORIENTED_EDGE('',*,*,#3842,.T.);
#5402=ORIENTED_EDGE('',*,*,#3843,.F.);
#5403=ORIENTED_EDGE('',*,*,#3844,.T.);
#5404=ORIENTED_EDGE('',*,*,#3840,.T.);
#5405=ORIENTED_EDGE('',*,*,#3845,.T.);
#5406=ORIENTED_EDGE('',*,*,#3846,.F.);
#5407=ORIENTED_EDGE('',*,*,#3847,.T.);
#5408=ORIENTED_EDGE('',*,*,#3843,.T.);
#5409=ORIENTED_EDGE('',*,*,#3848,.T.);
#5410=ORIENTED_EDGE('',*,*,#3849,.F.);
#5411=ORIENTED_EDGE('',*,*,#3850,.T.);
#5412=ORIENTED_EDGE('',*,*,#3846,.T.);
#5413=ORIENTED_EDGE('',*,*,#3851,.T.);
#5414=ORIENTED_EDGE('',*,*,#3852,.F.);
#5415=ORIENTED_EDGE('',*,*,#3853,.T.);
#5416=ORIENTED_EDGE('',*,*,#3849,.T.);
#5417=ORIENTED_EDGE('',*,*,#3854,.T.);
#5418=ORIENTED_EDGE('',*,*,#3855,.F.);
#5419=ORIENTED_EDGE('',*,*,#3856,.T.);
#5420=ORIENTED_EDGE('',*,*,#3852,.T.);
#5421=ORIENTED_EDGE('',*,*,#3857,.T.);
#5422=ORIENTED_EDGE('',*,*,#3858,.F.);
#5423=ORIENTED_EDGE('',*,*,#3859,.T.);
#5424=ORIENTED_EDGE('',*,*,#3855,.T.);
#5425=ORIENTED_EDGE('',*,*,#3860,.T.);
#5426=ORIENTED_EDGE('',*,*,#3861,.F.);
#5427=ORIENTED_EDGE('',*,*,#3862,.T.);
#5428=ORIENTED_EDGE('',*,*,#3858,.T.);
#5429=ORIENTED_EDGE('',*,*,#3863,.T.);
#5430=ORIENTED_EDGE('',*,*,#3864,.F.);
#5431=ORIENTED_EDGE('',*,*,#3865,.T.);
#5432=ORIENTED_EDGE('',*,*,#3861,.T.);
#5433=ORIENTED_EDGE('',*,*,#3866,.T.);
#5434=ORIENTED_EDGE('',*,*,#3867,.F.);
#5435=ORIENTED_EDGE('',*,*,#3868,.T.);
#5436=ORIENTED_EDGE('',*,*,#3864,.T.);
#5437=ORIENTED_EDGE('',*,*,#3869,.T.);
#5438=ORIENTED_EDGE('',*,*,#3870,.F.);
#5439=ORIENTED_EDGE('',*,*,#3871,.T.);
#5440=ORIENTED_EDGE('',*,*,#3867,.T.);
#5441=ORIENTED_EDGE('',*,*,#3872,.T.);
#5442=ORIENTED_EDGE('',*,*,#3873,.F.);
#5443=ORIENTED_EDGE('',*,*,#3874,.T.);
#5444=ORIENTED_EDGE('',*,*,#3870,.T.);
#5445=ORIENTED_EDGE('',*,*,#3875,.T.);
#5446=ORIENTED_EDGE('',*,*,#3876,.F.);
#5447=ORIENTED_EDGE('',*,*,#3877,.T.);
#5448=ORIENTED_EDGE('',*,*,#3873,.T.);
#5449=ORIENTED_EDGE('',*,*,#3878,.T.);
#5450=ORIENTED_EDGE('',*,*,#3879,.F.);
#5451=ORIENTED_EDGE('',*,*,#3880,.T.);
#5452=ORIENTED_EDGE('',*,*,#3881,.T.);
#5453=ORIENTED_EDGE('',*,*,#3882,.F.);
#5454=ORIENTED_EDGE('',*,*,#3883,.F.);
#5455=ORIENTED_EDGE('',*,*,#3884,.T.);
#5456=ORIENTED_EDGE('',*,*,#3879,.T.);
#5457=ORIENTED_EDGE('',*,*,#3885,.F.);
#5458=ORIENTED_EDGE('',*,*,#3886,.F.);
#5459=ORIENTED_EDGE('',*,*,#3887,.T.);
#5460=ORIENTED_EDGE('',*,*,#3883,.T.);
#5461=ORIENTED_EDGE('',*,*,#3888,.F.);
#5462=ORIENTED_EDGE('',*,*,#3889,.F.);
#5463=ORIENTED_EDGE('',*,*,#3890,.T.);
#5464=ORIENTED_EDGE('',*,*,#3886,.T.);
#5465=ORIENTED_EDGE('',*,*,#3891,.F.);
#5466=ORIENTED_EDGE('',*,*,#3892,.F.);
#5467=ORIENTED_EDGE('',*,*,#3893,.T.);
#5468=ORIENTED_EDGE('',*,*,#3889,.T.);
#5469=ORIENTED_EDGE('',*,*,#3894,.F.);
#5470=ORIENTED_EDGE('',*,*,#3895,.F.);
#5471=ORIENTED_EDGE('',*,*,#3896,.T.);
#5472=ORIENTED_EDGE('',*,*,#3892,.T.);
#5473=ORIENTED_EDGE('',*,*,#3897,.F.);
#5474=ORIENTED_EDGE('',*,*,#3898,.F.);
#5475=ORIENTED_EDGE('',*,*,#3899,.T.);
#5476=ORIENTED_EDGE('',*,*,#3895,.T.);
#5477=ORIENTED_EDGE('',*,*,#3900,.F.);
#5478=ORIENTED_EDGE('',*,*,#3901,.F.);
#5479=ORIENTED_EDGE('',*,*,#3902,.T.);
#5480=ORIENTED_EDGE('',*,*,#3898,.T.);
#5481=ORIENTED_EDGE('',*,*,#3903,.F.);
#5482=ORIENTED_EDGE('',*,*,#3904,.F.);
#5483=ORIENTED_EDGE('',*,*,#3905,.T.);
#5484=ORIENTED_EDGE('',*,*,#3901,.T.);
#5485=ORIENTED_EDGE('',*,*,#3906,.F.);
#5486=ORIENTED_EDGE('',*,*,#3907,.F.);
#5487=ORIENTED_EDGE('',*,*,#3908,.T.);
#5488=ORIENTED_EDGE('',*,*,#3904,.T.);
#5489=ORIENTED_EDGE('',*,*,#3909,.F.);
#5490=ORIENTED_EDGE('',*,*,#3910,.F.);
#5491=ORIENTED_EDGE('',*,*,#3911,.T.);
#5492=ORIENTED_EDGE('',*,*,#3907,.T.);
#5493=ORIENTED_EDGE('',*,*,#3912,.F.);
#5494=ORIENTED_EDGE('',*,*,#3913,.F.);
#5495=ORIENTED_EDGE('',*,*,#3914,.T.);
#5496=ORIENTED_EDGE('',*,*,#3910,.T.);
#5497=ORIENTED_EDGE('',*,*,#3915,.F.);
#5498=ORIENTED_EDGE('',*,*,#3916,.F.);
#5499=ORIENTED_EDGE('',*,*,#3917,.T.);
#5500=ORIENTED_EDGE('',*,*,#3913,.T.);
#5501=ORIENTED_EDGE('',*,*,#3918,.F.);
#5502=ORIENTED_EDGE('',*,*,#3919,.F.);
#5503=ORIENTED_EDGE('',*,*,#3920,.T.);
#5504=ORIENTED_EDGE('',*,*,#3916,.T.);
#5505=ORIENTED_EDGE('',*,*,#3921,.F.);
#5506=ORIENTED_EDGE('',*,*,#3922,.F.);
#5507=ORIENTED_EDGE('',*,*,#3923,.T.);
#5508=ORIENTED_EDGE('',*,*,#3919,.T.);
#5509=ORIENTED_EDGE('',*,*,#3924,.F.);
#5510=ORIENTED_EDGE('',*,*,#3925,.F.);
#5511=ORIENTED_EDGE('',*,*,#3926,.T.);
#5512=ORIENTED_EDGE('',*,*,#3922,.T.);
#5513=ORIENTED_EDGE('',*,*,#3927,.F.);
#5514=ORIENTED_EDGE('',*,*,#3928,.F.);
#5515=ORIENTED_EDGE('',*,*,#3929,.T.);
#5516=ORIENTED_EDGE('',*,*,#3925,.T.);
#5517=ORIENTED_EDGE('',*,*,#3930,.F.);
#5518=ORIENTED_EDGE('',*,*,#3931,.F.);
#5519=ORIENTED_EDGE('',*,*,#3932,.T.);
#5520=ORIENTED_EDGE('',*,*,#3928,.T.);
#5521=ORIENTED_EDGE('',*,*,#3933,.F.);
#5522=ORIENTED_EDGE('',*,*,#3934,.F.);
#5523=ORIENTED_EDGE('',*,*,#3935,.T.);
#5524=ORIENTED_EDGE('',*,*,#3931,.T.);
#5525=ORIENTED_EDGE('',*,*,#3936,.F.);
#5526=ORIENTED_EDGE('',*,*,#3937,.F.);
#5527=ORIENTED_EDGE('',*,*,#3938,.T.);
#5528=ORIENTED_EDGE('',*,*,#3934,.T.);
#5529=ORIENTED_EDGE('',*,*,#3939,.F.);
#5530=ORIENTED_EDGE('',*,*,#3940,.F.);
#5531=ORIENTED_EDGE('',*,*,#3941,.T.);
#5532=ORIENTED_EDGE('',*,*,#3937,.T.);
#5533=ORIENTED_EDGE('',*,*,#3942,.F.);
#5534=ORIENTED_EDGE('',*,*,#3943,.F.);
#5535=ORIENTED_EDGE('',*,*,#3944,.T.);
#5536=ORIENTED_EDGE('',*,*,#3940,.T.);
#5537=ORIENTED_EDGE('',*,*,#3945,.F.);
#5538=ORIENTED_EDGE('',*,*,#3946,.F.);
#5539=ORIENTED_EDGE('',*,*,#3947,.T.);
#5540=ORIENTED_EDGE('',*,*,#3943,.T.);
#5541=ORIENTED_EDGE('',*,*,#3948,.F.);
#5542=ORIENTED_EDGE('',*,*,#3949,.F.);
#5543=ORIENTED_EDGE('',*,*,#3950,.T.);
#5544=ORIENTED_EDGE('',*,*,#3946,.T.);
#5545=ORIENTED_EDGE('',*,*,#3951,.F.);
#5546=ORIENTED_EDGE('',*,*,#3952,.F.);
#5547=ORIENTED_EDGE('',*,*,#3953,.T.);
#5548=ORIENTED_EDGE('',*,*,#3949,.T.);
#5549=ORIENTED_EDGE('',*,*,#3954,.F.);
#5550=ORIENTED_EDGE('',*,*,#3955,.F.);
#5551=ORIENTED_EDGE('',*,*,#3956,.T.);
#5552=ORIENTED_EDGE('',*,*,#3952,.T.);
#5553=ORIENTED_EDGE('',*,*,#3957,.F.);
#5554=ORIENTED_EDGE('',*,*,#3958,.F.);
#5555=ORIENTED_EDGE('',*,*,#3959,.T.);
#5556=ORIENTED_EDGE('',*,*,#3955,.T.);
#5557=ORIENTED_EDGE('',*,*,#3960,.F.);
#5558=ORIENTED_EDGE('',*,*,#3961,.F.);
#5559=ORIENTED_EDGE('',*,*,#3962,.T.);
#5560=ORIENTED_EDGE('',*,*,#3958,.T.);
#5561=ORIENTED_EDGE('',*,*,#3963,.F.);
#5562=ORIENTED_EDGE('',*,*,#3964,.F.);
#5563=ORIENTED_EDGE('',*,*,#3965,.T.);
#5564=ORIENTED_EDGE('',*,*,#3961,.T.);
#5565=ORIENTED_EDGE('',*,*,#3966,.F.);
#5566=ORIENTED_EDGE('',*,*,#3967,.F.);
#5567=ORIENTED_EDGE('',*,*,#3968,.T.);
#5568=ORIENTED_EDGE('',*,*,#3964,.T.);
#5569=ORIENTED_EDGE('',*,*,#3969,.F.);
#5570=ORIENTED_EDGE('',*,*,#3970,.F.);
#5571=ORIENTED_EDGE('',*,*,#3881,.F.);
#5572=ORIENTED_EDGE('',*,*,#3971,.F.);
#5573=ORIENTED_EDGE('',*,*,#3972,.F.);
#5574=ORIENTED_EDGE('',*,*,#3973,.F.);
#5575=ORIENTED_EDGE('',*,*,#3974,.T.);
#5576=ORIENTED_EDGE('',*,*,#3975,.F.);
#5577=ORIENTED_EDGE('',*,*,#3974,.F.);
#5578=ORIENTED_EDGE('',*,*,#3971,.T.);
#5579=ORIENTED_EDGE('',*,*,#3880,.F.);
#5580=ORIENTED_EDGE('',*,*,#3884,.F.);
#5581=ORIENTED_EDGE('',*,*,#3887,.F.);
#5582=ORIENTED_EDGE('',*,*,#3890,.F.);
#5583=ORIENTED_EDGE('',*,*,#3893,.F.);
#5584=ORIENTED_EDGE('',*,*,#3896,.F.);
#5585=ORIENTED_EDGE('',*,*,#3899,.F.);
#5586=ORIENTED_EDGE('',*,*,#3902,.F.);
#5587=ORIENTED_EDGE('',*,*,#3905,.F.);
#5588=ORIENTED_EDGE('',*,*,#3908,.F.);
#5589=ORIENTED_EDGE('',*,*,#3911,.F.);
#5590=ORIENTED_EDGE('',*,*,#3914,.F.);
#5591=ORIENTED_EDGE('',*,*,#3917,.F.);
#5592=ORIENTED_EDGE('',*,*,#3920,.F.);
#5593=ORIENTED_EDGE('',*,*,#3923,.F.);
#5594=ORIENTED_EDGE('',*,*,#3926,.F.);
#5595=ORIENTED_EDGE('',*,*,#3929,.F.);
#5596=ORIENTED_EDGE('',*,*,#3932,.F.);
#5597=ORIENTED_EDGE('',*,*,#3935,.F.);
#5598=ORIENTED_EDGE('',*,*,#3938,.F.);
#5599=ORIENTED_EDGE('',*,*,#3941,.F.);
#5600=ORIENTED_EDGE('',*,*,#3944,.F.);
#5601=ORIENTED_EDGE('',*,*,#3947,.F.);
#5602=ORIENTED_EDGE('',*,*,#3950,.F.);
#5603=ORIENTED_EDGE('',*,*,#3953,.F.);
#5604=ORIENTED_EDGE('',*,*,#3956,.F.);
#5605=ORIENTED_EDGE('',*,*,#3959,.F.);
#5606=ORIENTED_EDGE('',*,*,#3962,.F.);
#5607=ORIENTED_EDGE('',*,*,#3965,.F.);
#5608=ORIENTED_EDGE('',*,*,#3968,.F.);
#5609=ORIENTED_EDGE('',*,*,#3976,.F.);
#5610=ORIENTED_EDGE('',*,*,#3977,.F.);
#5611=ORIENTED_EDGE('',*,*,#3789,.F.);
#5612=ORIENTED_EDGE('',*,*,#3793,.F.);
#5613=ORIENTED_EDGE('',*,*,#3796,.F.);
#5614=ORIENTED_EDGE('',*,*,#3799,.F.);
#5615=ORIENTED_EDGE('',*,*,#3802,.F.);
#5616=ORIENTED_EDGE('',*,*,#3805,.F.);
#5617=ORIENTED_EDGE('',*,*,#3808,.F.);
#5618=ORIENTED_EDGE('',*,*,#3811,.F.);
#5619=ORIENTED_EDGE('',*,*,#3814,.F.);
#5620=ORIENTED_EDGE('',*,*,#3817,.F.);
#5621=ORIENTED_EDGE('',*,*,#3820,.F.);
#5622=ORIENTED_EDGE('',*,*,#3823,.F.);
#5623=ORIENTED_EDGE('',*,*,#3826,.F.);
#5624=ORIENTED_EDGE('',*,*,#3829,.F.);
#5625=ORIENTED_EDGE('',*,*,#3832,.F.);
#5626=ORIENTED_EDGE('',*,*,#3835,.F.);
#5627=ORIENTED_EDGE('',*,*,#3838,.F.);
#5628=ORIENTED_EDGE('',*,*,#3841,.F.);
#5629=ORIENTED_EDGE('',*,*,#3844,.F.);
#5630=ORIENTED_EDGE('',*,*,#3847,.F.);
#5631=ORIENTED_EDGE('',*,*,#3850,.F.);
#5632=ORIENTED_EDGE('',*,*,#3853,.F.);
#5633=ORIENTED_EDGE('',*,*,#3856,.F.);
#5634=ORIENTED_EDGE('',*,*,#3859,.F.);
#5635=ORIENTED_EDGE('',*,*,#3862,.F.);
#5636=ORIENTED_EDGE('',*,*,#3865,.F.);
#5637=ORIENTED_EDGE('',*,*,#3868,.F.);
#5638=ORIENTED_EDGE('',*,*,#3871,.F.);
#5639=ORIENTED_EDGE('',*,*,#3874,.F.);
#5640=ORIENTED_EDGE('',*,*,#3877,.F.);
#5641=ORIENTED_EDGE('',*,*,#3978,.F.);
#5642=ORIENTED_EDGE('',*,*,#3967,.T.);
#5643=ORIENTED_EDGE('',*,*,#3979,.F.);
#5644=ORIENTED_EDGE('',*,*,#3980,.F.);
#5645=ORIENTED_EDGE('',*,*,#3976,.T.);
#5646=ORIENTED_EDGE('',*,*,#3970,.T.);
#5647=ORIENTED_EDGE('',*,*,#3973,.T.);
#5648=ORIENTED_EDGE('',*,*,#3981,.F.);
#5649=ORIENTED_EDGE('',*,*,#3878,.F.);
#5650=ORIENTED_EDGE('',*,*,#3875,.F.);
#5651=ORIENTED_EDGE('',*,*,#3872,.F.);
#5652=ORIENTED_EDGE('',*,*,#3869,.F.);
#5653=ORIENTED_EDGE('',*,*,#3866,.F.);
#5654=ORIENTED_EDGE('',*,*,#3863,.F.);
#5655=ORIENTED_EDGE('',*,*,#3860,.F.);
#5656=ORIENTED_EDGE('',*,*,#3857,.F.);
#5657=ORIENTED_EDGE('',*,*,#3854,.F.);
#5658=ORIENTED_EDGE('',*,*,#3851,.F.);
#5659=ORIENTED_EDGE('',*,*,#3848,.F.);
#5660=ORIENTED_EDGE('',*,*,#3845,.F.);
#5661=ORIENTED_EDGE('',*,*,#3842,.F.);
#5662=ORIENTED_EDGE('',*,*,#3839,.F.);
#5663=ORIENTED_EDGE('',*,*,#3836,.F.);
#5664=ORIENTED_EDGE('',*,*,#3833,.F.);
#5665=ORIENTED_EDGE('',*,*,#3830,.F.);
#5666=ORIENTED_EDGE('',*,*,#3827,.F.);
#5667=ORIENTED_EDGE('',*,*,#3824,.F.);
#5668=ORIENTED_EDGE('',*,*,#3821,.F.);
#5669=ORIENTED_EDGE('',*,*,#3818,.F.);
#5670=ORIENTED_EDGE('',*,*,#3815,.F.);
#5671=ORIENTED_EDGE('',*,*,#3812,.F.);
#5672=ORIENTED_EDGE('',*,*,#3809,.F.);
#5673=ORIENTED_EDGE('',*,*,#3806,.F.);
#5674=ORIENTED_EDGE('',*,*,#3803,.F.);
#5675=ORIENTED_EDGE('',*,*,#3800,.F.);
#5676=ORIENTED_EDGE('',*,*,#3797,.F.);
#5677=ORIENTED_EDGE('',*,*,#3794,.F.);
#5678=ORIENTED_EDGE('',*,*,#3791,.F.);
#5679=ORIENTED_EDGE('',*,*,#3982,.F.);
#5680=ORIENTED_EDGE('',*,*,#3979,.T.);
#5681=ORIENTED_EDGE('',*,*,#3969,.T.);
#5682=ORIENTED_EDGE('',*,*,#3966,.T.);
#5683=ORIENTED_EDGE('',*,*,#3963,.T.);
#5684=ORIENTED_EDGE('',*,*,#3960,.T.);
#5685=ORIENTED_EDGE('',*,*,#3957,.T.);
#5686=ORIENTED_EDGE('',*,*,#3954,.T.);
#5687=ORIENTED_EDGE('',*,*,#3951,.T.);
#5688=ORIENTED_EDGE('',*,*,#3948,.T.);
#5689=ORIENTED_EDGE('',*,*,#3945,.T.);
#5690=ORIENTED_EDGE('',*,*,#3942,.T.);
#5691=ORIENTED_EDGE('',*,*,#3939,.T.);
#5692=ORIENTED_EDGE('',*,*,#3936,.T.);
#5693=ORIENTED_EDGE('',*,*,#3933,.T.);
#5694=ORIENTED_EDGE('',*,*,#3930,.T.);
#5695=ORIENTED_EDGE('',*,*,#3927,.T.);
#5696=ORIENTED_EDGE('',*,*,#3924,.T.);
#5697=ORIENTED_EDGE('',*,*,#3921,.T.);
#5698=ORIENTED_EDGE('',*,*,#3918,.T.);
#5699=ORIENTED_EDGE('',*,*,#3915,.T.);
#5700=ORIENTED_EDGE('',*,*,#3912,.T.);
#5701=ORIENTED_EDGE('',*,*,#3909,.T.);
#5702=ORIENTED_EDGE('',*,*,#3906,.T.);
#5703=ORIENTED_EDGE('',*,*,#3903,.T.);
#5704=ORIENTED_EDGE('',*,*,#3900,.T.);
#5705=ORIENTED_EDGE('',*,*,#3897,.T.);
#5706=ORIENTED_EDGE('',*,*,#3894,.T.);
#5707=ORIENTED_EDGE('',*,*,#3891,.T.);
#5708=ORIENTED_EDGE('',*,*,#3888,.T.);
#5709=ORIENTED_EDGE('',*,*,#3885,.T.);
#5710=ORIENTED_EDGE('',*,*,#3882,.T.);
#5711=ORIENTED_EDGE('',*,*,#3876,.T.);
#5712=ORIENTED_EDGE('',*,*,#3981,.T.);
#5713=ORIENTED_EDGE('',*,*,#3972,.T.);
#5714=ORIENTED_EDGE('',*,*,#3978,.T.);
#5715=ORIENTED_EDGE('',*,*,#3983,.F.);
#5716=ORIENTED_EDGE('',*,*,#3984,.T.);
#5717=ORIENTED_EDGE('',*,*,#3985,.T.);
#5718=ORIENTED_EDGE('',*,*,#3986,.F.);
#5719=ORIENTED_EDGE('',*,*,#3987,.F.);
#5720=ORIENTED_EDGE('',*,*,#3988,.T.);
#5721=ORIENTED_EDGE('',*,*,#3989,.T.);
#5722=ORIENTED_EDGE('',*,*,#3984,.F.);
#5723=ORIENTED_EDGE('',*,*,#3990,.F.);
#5724=ORIENTED_EDGE('',*,*,#3991,.T.);
#5725=ORIENTED_EDGE('',*,*,#3992,.T.);
#5726=ORIENTED_EDGE('',*,*,#3988,.F.);
#5727=ORIENTED_EDGE('',*,*,#3993,.F.);
#5728=ORIENTED_EDGE('',*,*,#3994,.T.);
#5729=ORIENTED_EDGE('',*,*,#3995,.T.);
#5730=ORIENTED_EDGE('',*,*,#3991,.F.);
#5731=ORIENTED_EDGE('',*,*,#3996,.F.);
#5732=ORIENTED_EDGE('',*,*,#3997,.T.);
#5733=ORIENTED_EDGE('',*,*,#3998,.T.);
#5734=ORIENTED_EDGE('',*,*,#3994,.F.);
#5735=ORIENTED_EDGE('',*,*,#3999,.F.);
#5736=ORIENTED_EDGE('',*,*,#3986,.T.);
#5737=ORIENTED_EDGE('',*,*,#4000,.T.);
#5738=ORIENTED_EDGE('',*,*,#3997,.F.);
#5739=ORIENTED_EDGE('',*,*,#4000,.F.);
#5740=ORIENTED_EDGE('',*,*,#3985,.F.);
#5741=ORIENTED_EDGE('',*,*,#3989,.F.);
#5742=ORIENTED_EDGE('',*,*,#3992,.F.);
#5743=ORIENTED_EDGE('',*,*,#3995,.F.);
#5744=ORIENTED_EDGE('',*,*,#3998,.F.);
#5745=ORIENTED_EDGE('',*,*,#4001,.T.);
#5746=ORIENTED_EDGE('',*,*,#3977,.T.);
#5747=ORIENTED_EDGE('',*,*,#3980,.T.);
#5748=ORIENTED_EDGE('',*,*,#3982,.T.);
#5749=ORIENTED_EDGE('',*,*,#3790,.F.);
#5750=ORIENTED_EDGE('',*,*,#4001,.F.);
#5751=ORIENTED_EDGE('',*,*,#4002,.T.);
#5752=ORIENTED_EDGE('',*,*,#4003,.T.);
#5753=ORIENTED_EDGE('',*,*,#4002,.F.);
#5754=ORIENTED_EDGE('',*,*,#4003,.F.);
#5755=ORIENTED_EDGE('',*,*,#3983,.T.);
#5756=ORIENTED_EDGE('',*,*,#3999,.T.);
#5757=ORIENTED_EDGE('',*,*,#3996,.T.);
#5758=ORIENTED_EDGE('',*,*,#3993,.T.);
#5759=ORIENTED_EDGE('',*,*,#3990,.T.);
#5760=ORIENTED_EDGE('',*,*,#3987,.T.);
#5761=ORIENTED_EDGE('',*,*,#3975,.T.);
#5762=ORIENTED_EDGE('',*,*,#4004,.T.);
#5763=ORIENTED_EDGE('',*,*,#4005,.F.);
#5764=ORIENTED_EDGE('',*,*,#4006,.T.);
#5765=ORIENTED_EDGE('',*,*,#4007,.T.);
#5766=ORIENTED_EDGE('',*,*,#4008,.T.);
#5767=ORIENTED_EDGE('',*,*,#4009,.F.);
#5768=ORIENTED_EDGE('',*,*,#4004,.F.);
#5769=ORIENTED_EDGE('',*,*,#4010,.T.);
#5770=ORIENTED_EDGE('',*,*,#4011,.T.);
#5771=ORIENTED_EDGE('',*,*,#4012,.T.);
#5772=ORIENTED_EDGE('',*,*,#4007,.F.);
#5773=ORIENTED_EDGE('',*,*,#4013,.T.);
#5774=ORIENTED_EDGE('',*,*,#4014,.T.);
#5775=ORIENTED_EDGE('',*,*,#4015,.T.);
#5776=ORIENTED_EDGE('',*,*,#4011,.F.);
#5777=ORIENTED_EDGE('',*,*,#4016,.T.);
#5778=ORIENTED_EDGE('',*,*,#4017,.F.);
#5779=ORIENTED_EDGE('',*,*,#4018,.T.);
#5780=ORIENTED_EDGE('',*,*,#4019,.F.);
#5781=ORIENTED_EDGE('',*,*,#4020,.T.);
#5782=ORIENTED_EDGE('',*,*,#4021,.T.);
#5783=ORIENTED_EDGE('',*,*,#4022,.T.);
#5784=ORIENTED_EDGE('',*,*,#4023,.F.);
#5785=ORIENTED_EDGE('',*,*,#4024,.F.);
#5786=ORIENTED_EDGE('',*,*,#4025,.T.);
#5787=ORIENTED_EDGE('',*,*,#4026,.T.);
#5788=ORIENTED_EDGE('',*,*,#4021,.F.);
#5789=ORIENTED_EDGE('',*,*,#4027,.F.);
#5790=ORIENTED_EDGE('',*,*,#4028,.T.);
#5791=ORIENTED_EDGE('',*,*,#4029,.T.);
#5792=ORIENTED_EDGE('',*,*,#4025,.F.);
#5793=ORIENTED_EDGE('',*,*,#4030,.F.);
#5794=ORIENTED_EDGE('',*,*,#4031,.T.);
#5795=ORIENTED_EDGE('',*,*,#4032,.T.);
#5796=ORIENTED_EDGE('',*,*,#4028,.F.);
#5797=ORIENTED_EDGE('',*,*,#4033,.F.);
#5798=ORIENTED_EDGE('',*,*,#4034,.F.);
#5799=ORIENTED_EDGE('',*,*,#4035,.F.);
#5800=ORIENTED_EDGE('',*,*,#4036,.F.);
#5801=ORIENTED_EDGE('',*,*,#4037,.T.);
#5802=ORIENTED_EDGE('',*,*,#4034,.T.);
#5803=ORIENTED_EDGE('',*,*,#4038,.T.);
#5804=ORIENTED_EDGE('',*,*,#4031,.F.);
#5805=ORIENTED_EDGE('',*,*,#4039,.F.);
#5806=ORIENTED_EDGE('',*,*,#4040,.F.);
#5807=ORIENTED_EDGE('',*,*,#4022,.F.);
#5808=ORIENTED_EDGE('',*,*,#4026,.F.);
#5809=ORIENTED_EDGE('',*,*,#4029,.F.);
#5810=ORIENTED_EDGE('',*,*,#4032,.F.);
#5811=ORIENTED_EDGE('',*,*,#4038,.F.);
#5812=ORIENTED_EDGE('',*,*,#4037,.F.);
#5813=ORIENTED_EDGE('',*,*,#4041,.F.);
#5814=ORIENTED_EDGE('',*,*,#4018,.F.);
#5815=ORIENTED_EDGE('',*,*,#4042,.F.);
#5816=ORIENTED_EDGE('',*,*,#4016,.F.);
#5817=ORIENTED_EDGE('',*,*,#4013,.F.);
#5818=ORIENTED_EDGE('',*,*,#4010,.F.);
#5819=ORIENTED_EDGE('',*,*,#4006,.F.);
#5820=ORIENTED_EDGE('',*,*,#4043,.F.);
#5821=ORIENTED_EDGE('',*,*,#4008,.F.);
#5822=ORIENTED_EDGE('',*,*,#4012,.F.);
#5823=ORIENTED_EDGE('',*,*,#4015,.F.);
#5824=ORIENTED_EDGE('',*,*,#4044,.F.);
#5825=ORIENTED_EDGE('',*,*,#4020,.F.);
#5826=ORIENTED_EDGE('',*,*,#4045,.F.);
#5827=ORIENTED_EDGE('',*,*,#4035,.T.);
#5828=ORIENTED_EDGE('',*,*,#4039,.T.);
#5829=ORIENTED_EDGE('',*,*,#4033,.T.);
#5830=ORIENTED_EDGE('',*,*,#4030,.T.);
#5831=ORIENTED_EDGE('',*,*,#4027,.T.);
#5832=ORIENTED_EDGE('',*,*,#4024,.T.);
#5833=ORIENTED_EDGE('',*,*,#4046,.T.);
#5834=ORIENTED_EDGE('',*,*,#4047,.T.);
#5835=ORIENTED_EDGE('',*,*,#4048,.T.);
#5836=ORIENTED_EDGE('',*,*,#4049,.T.);
#5837=ORIENTED_EDGE('',*,*,#4050,.T.);
#5838=ORIENTED_EDGE('',*,*,#4051,.T.);
#5839=ORIENTED_EDGE('',*,*,#4041,.T.);
#5840=ORIENTED_EDGE('',*,*,#4036,.T.);
#5841=ORIENTED_EDGE('',*,*,#4045,.T.);
#5842=ORIENTED_EDGE('',*,*,#4019,.T.);
#5843=ORIENTED_EDGE('',*,*,#4017,.T.);
#5844=ORIENTED_EDGE('',*,*,#4044,.T.);
#5845=ORIENTED_EDGE('',*,*,#4014,.F.);
#5846=ORIENTED_EDGE('',*,*,#4042,.T.);
#5847=ORIENTED_EDGE('',*,*,#4052,.T.);
#5848=ORIENTED_EDGE('',*,*,#4053,.T.);
#5849=ORIENTED_EDGE('',*,*,#4051,.F.);
#5850=ORIENTED_EDGE('',*,*,#4054,.F.);
#5851=ORIENTED_EDGE('',*,*,#4055,.T.);
#5852=ORIENTED_EDGE('',*,*,#4054,.T.);
#5853=ORIENTED_EDGE('',*,*,#4050,.F.);
#5854=ORIENTED_EDGE('',*,*,#4056,.F.);
#5855=ORIENTED_EDGE('',*,*,#4057,.T.);
#5856=ORIENTED_EDGE('',*,*,#4056,.T.);
#5857=ORIENTED_EDGE('',*,*,#4049,.F.);
#5858=ORIENTED_EDGE('',*,*,#4058,.F.);
#5859=ORIENTED_EDGE('',*,*,#4059,.T.);
#5860=ORIENTED_EDGE('',*,*,#4058,.T.);
#5861=ORIENTED_EDGE('',*,*,#4048,.F.);
#5862=ORIENTED_EDGE('',*,*,#4060,.F.);
#5863=ORIENTED_EDGE('',*,*,#4061,.T.);
#5864=ORIENTED_EDGE('',*,*,#4060,.T.);
#5865=ORIENTED_EDGE('',*,*,#4047,.F.);
#5866=ORIENTED_EDGE('',*,*,#4062,.F.);
#5867=ORIENTED_EDGE('',*,*,#4063,.T.);
#5868=ORIENTED_EDGE('',*,*,#4062,.T.);
#5869=ORIENTED_EDGE('',*,*,#4046,.F.);
#5870=ORIENTED_EDGE('',*,*,#4053,.F.);
#5871=ORIENTED_EDGE('',*,*,#4063,.F.);
#5872=ORIENTED_EDGE('',*,*,#4052,.F.);
#5873=ORIENTED_EDGE('',*,*,#4055,.F.);
#5874=ORIENTED_EDGE('',*,*,#4057,.F.);
#5875=ORIENTED_EDGE('',*,*,#4059,.F.);
#5876=ORIENTED_EDGE('',*,*,#4061,.F.);
#5877=ORIENTED_EDGE('',*,*,#4040,.T.);
#5878=ORIENTED_EDGE('',*,*,#4005,.T.);
#5879=ORIENTED_EDGE('',*,*,#4009,.T.);
#5880=ORIENTED_EDGE('',*,*,#4043,.T.);
#5881=ORIENTED_EDGE('',*,*,#4023,.T.);
#5882=ORIENTED_EDGE('',*,*,#4064,.F.);
#5883=ORIENTED_EDGE('',*,*,#4065,.T.);
#5884=ORIENTED_EDGE('',*,*,#4066,.F.);
#5885=ORIENTED_EDGE('',*,*,#4065,.F.);
#5886=ORIENTED_EDGE('',*,*,#4067,.F.);
#5887=ORIENTED_EDGE('',*,*,#4068,.T.);
#5888=ORIENTED_EDGE('',*,*,#4069,.F.);
#5889=ORIENTED_EDGE('',*,*,#4068,.F.);
#5890=ORIENTED_EDGE('',*,*,#4070,.T.);
#5891=ORIENTED_EDGE('',*,*,#4071,.T.);
#5892=ORIENTED_EDGE('',*,*,#4072,.F.);
#5893=ORIENTED_EDGE('',*,*,#4073,.T.);
#5894=ORIENTED_EDGE('',*,*,#4070,.F.);
#5895=ORIENTED_EDGE('',*,*,#4073,.F.);
#5896=ORIENTED_EDGE('',*,*,#4072,.T.);
#5897=ORIENTED_EDGE('',*,*,#4074,.T.);
#5898=ORIENTED_EDGE('',*,*,#4075,.T.);
#5899=ORIENTED_EDGE('',*,*,#4076,.F.);
#5900=ORIENTED_EDGE('',*,*,#4077,.T.);
#5901=ORIENTED_EDGE('',*,*,#4074,.F.);
#5902=ORIENTED_EDGE('',*,*,#4077,.F.);
#5903=ORIENTED_EDGE('',*,*,#4076,.T.);
#5904=ORIENTED_EDGE('',*,*,#4078,.T.);
#5905=ORIENTED_EDGE('',*,*,#4079,.T.);
#5906=ORIENTED_EDGE('',*,*,#4080,.F.);
#5907=ORIENTED_EDGE('',*,*,#4081,.T.);
#5908=ORIENTED_EDGE('',*,*,#4078,.F.);
#5909=ORIENTED_EDGE('',*,*,#4081,.F.);
#5910=ORIENTED_EDGE('',*,*,#4080,.T.);
#5911=ORIENTED_EDGE('',*,*,#4082,.T.);
#5912=ORIENTED_EDGE('',*,*,#4083,.T.);
#5913=ORIENTED_EDGE('',*,*,#4084,.F.);
#5914=ORIENTED_EDGE('',*,*,#4085,.T.);
#5915=ORIENTED_EDGE('',*,*,#4082,.F.);
#5916=ORIENTED_EDGE('',*,*,#4085,.F.);
#5917=ORIENTED_EDGE('',*,*,#4084,.T.);
#5918=ORIENTED_EDGE('',*,*,#4071,.F.);
#5919=ORIENTED_EDGE('',*,*,#4086,.T.);
#5920=ORIENTED_EDGE('',*,*,#4087,.F.);
#5921=ORIENTED_EDGE('',*,*,#4086,.F.);
#5922=ORIENTED_EDGE('',*,*,#4075,.F.);
#5923=ORIENTED_EDGE('',*,*,#4088,.T.);
#5924=ORIENTED_EDGE('',*,*,#4089,.F.);
#5925=ORIENTED_EDGE('',*,*,#4088,.F.);
#5926=ORIENTED_EDGE('',*,*,#4079,.F.);
#5927=ORIENTED_EDGE('',*,*,#4090,.T.);
#5928=ORIENTED_EDGE('',*,*,#4091,.F.);
#5929=ORIENTED_EDGE('',*,*,#4090,.F.);
#5930=ORIENTED_EDGE('',*,*,#4083,.F.);
#5931=ORIENTED_EDGE('',*,*,#4092,.T.);
#5932=ORIENTED_EDGE('',*,*,#4093,.F.);
#5933=ORIENTED_EDGE('',*,*,#4092,.F.);
#5934=ORIENTED_EDGE('',*,*,#4094,.T.);
#5935=ORIENTED_EDGE('',*,*,#4095,.T.);
#5936=ORIENTED_EDGE('',*,*,#4096,.T.);
#5937=ORIENTED_EDGE('',*,*,#4097,.T.);
#5938=ORIENTED_EDGE('',*,*,#4098,.T.);
#5939=ORIENTED_EDGE('',*,*,#4099,.T.);
#5940=ORIENTED_EDGE('',*,*,#4094,.F.);
#5941=ORIENTED_EDGE('',*,*,#4100,.T.);
#5942=ORIENTED_EDGE('',*,*,#4101,.T.);
#5943=ORIENTED_EDGE('',*,*,#4102,.T.);
#5944=ORIENTED_EDGE('',*,*,#4098,.F.);
#5945=ORIENTED_EDGE('',*,*,#4103,.T.);
#5946=ORIENTED_EDGE('',*,*,#4104,.T.);
#5947=ORIENTED_EDGE('',*,*,#4105,.T.);
#5948=ORIENTED_EDGE('',*,*,#4101,.F.);
#5949=ORIENTED_EDGE('',*,*,#4106,.T.);
#5950=ORIENTED_EDGE('',*,*,#4107,.T.);
#5951=ORIENTED_EDGE('',*,*,#4108,.T.);
#5952=ORIENTED_EDGE('',*,*,#4104,.F.);
#5953=ORIENTED_EDGE('',*,*,#4109,.T.);
#5954=ORIENTED_EDGE('',*,*,#4110,.T.);
#5955=ORIENTED_EDGE('',*,*,#4111,.T.);
#5956=ORIENTED_EDGE('',*,*,#4107,.F.);
#5957=ORIENTED_EDGE('',*,*,#4112,.T.);
#5958=ORIENTED_EDGE('',*,*,#4113,.T.);
#5959=ORIENTED_EDGE('',*,*,#4114,.T.);
#5960=ORIENTED_EDGE('',*,*,#4110,.F.);
#5961=ORIENTED_EDGE('',*,*,#4115,.T.);
#5962=ORIENTED_EDGE('',*,*,#4096,.F.);
#5963=ORIENTED_EDGE('',*,*,#4116,.T.);
#5964=ORIENTED_EDGE('',*,*,#4113,.F.);
#5965=ORIENTED_EDGE('',*,*,#4117,.T.);
#5966=ORIENTED_EDGE('',*,*,#4111,.F.);
#5967=ORIENTED_EDGE('',*,*,#4118,.F.);
#5968=ORIENTED_EDGE('',*,*,#4119,.F.);
#5969=ORIENTED_EDGE('',*,*,#4120,.F.);
#5970=ORIENTED_EDGE('',*,*,#4114,.F.);
#5971=ORIENTED_EDGE('',*,*,#4121,.T.);
#5972=ORIENTED_EDGE('',*,*,#4122,.T.);
#5973=ORIENTED_EDGE('',*,*,#4118,.T.);
#5974=ORIENTED_EDGE('',*,*,#4116,.F.);
#5975=ORIENTED_EDGE('',*,*,#4123,.F.);
#5976=ORIENTED_EDGE('',*,*,#4124,.F.);
#5977=ORIENTED_EDGE('',*,*,#4121,.F.);
#5978=ORIENTED_EDGE('',*,*,#4095,.F.);
#5979=ORIENTED_EDGE('',*,*,#4125,.T.);
#5980=ORIENTED_EDGE('',*,*,#4126,.T.);
#5981=ORIENTED_EDGE('',*,*,#4123,.T.);
#5982=ORIENTED_EDGE('',*,*,#4097,.F.);
#5983=ORIENTED_EDGE('',*,*,#4117,.F.);
#5984=ORIENTED_EDGE('',*,*,#4115,.F.);
#5985=ORIENTED_EDGE('',*,*,#4112,.F.);
#5986=ORIENTED_EDGE('',*,*,#4109,.F.);
#5987=ORIENTED_EDGE('',*,*,#4106,.F.);
#5988=ORIENTED_EDGE('',*,*,#4103,.F.);
#5989=ORIENTED_EDGE('',*,*,#4100,.F.);
#5990=ORIENTED_EDGE('',*,*,#4064,.T.);
#5991=ORIENTED_EDGE('',*,*,#4067,.T.);
#5992=ORIENTED_EDGE('',*,*,#4099,.F.);
#5993=ORIENTED_EDGE('',*,*,#4127,.F.);
#5994=ORIENTED_EDGE('',*,*,#4128,.F.);
#5995=ORIENTED_EDGE('',*,*,#4125,.F.);
#5996=ORIENTED_EDGE('',*,*,#4108,.F.);
#5997=ORIENTED_EDGE('',*,*,#4120,.T.);
#5998=ORIENTED_EDGE('',*,*,#4129,.T.);
#5999=ORIENTED_EDGE('',*,*,#4130,.T.);
#6000=ORIENTED_EDGE('',*,*,#4102,.F.);
#6001=ORIENTED_EDGE('',*,*,#4131,.T.);
#6002=ORIENTED_EDGE('',*,*,#4132,.T.);
#6003=ORIENTED_EDGE('',*,*,#4127,.T.);
#6004=ORIENTED_EDGE('',*,*,#4126,.F.);
#6005=ORIENTED_EDGE('',*,*,#4128,.T.);
#6006=ORIENTED_EDGE('',*,*,#4132,.F.);
#6007=ORIENTED_EDGE('',*,*,#4133,.T.);
#6008=ORIENTED_EDGE('',*,*,#4129,.F.);
#6009=ORIENTED_EDGE('',*,*,#4119,.T.);
#6010=ORIENTED_EDGE('',*,*,#4122,.F.);
#6011=ORIENTED_EDGE('',*,*,#4124,.T.);
#6012=ORIENTED_EDGE('',*,*,#4066,.T.);
#6013=ORIENTED_EDGE('',*,*,#4069,.T.);
#6014=ORIENTED_EDGE('',*,*,#4087,.T.);
#6015=ORIENTED_EDGE('',*,*,#4089,.T.);
#6016=ORIENTED_EDGE('',*,*,#4091,.T.);
#6017=ORIENTED_EDGE('',*,*,#4093,.T.);
#6018=ORIENTED_EDGE('',*,*,#4105,.F.);
#6019=ORIENTED_EDGE('',*,*,#4130,.F.);
#6020=ORIENTED_EDGE('',*,*,#4133,.F.);
#6021=ORIENTED_EDGE('',*,*,#4131,.F.);
#6022=ORIENTED_EDGE('',*,*,#4134,.F.);
#6023=ORIENTED_EDGE('',*,*,#4135,.T.);
#6024=ORIENTED_EDGE('',*,*,#4136,.T.);
#6025=ORIENTED_EDGE('',*,*,#4135,.F.);
#6026=ORIENTED_EDGE('',*,*,#4137,.F.);
#6027=ORIENTED_EDGE('',*,*,#4138,.T.);
#6028=ORIENTED_EDGE('',*,*,#4139,.T.);
#6029=ORIENTED_EDGE('',*,*,#4138,.F.);
#6030=ORIENTED_EDGE('',*,*,#4137,.T.);
#6031=ORIENTED_EDGE('',*,*,#4134,.T.);
#6032=ORIENTED_EDGE('',*,*,#4139,.F.);
#6033=ORIENTED_EDGE('',*,*,#4136,.F.);
#6034=CYLINDRICAL_SURFACE('',#6655,0.17);
#6035=CYLINDRICAL_SURFACE('',#6658,0.17);
#6036=CYLINDRICAL_SURFACE('',#6661,0.41);
#6037=CYLINDRICAL_SURFACE('',#6681,1.4);
#6038=CYLINDRICAL_SURFACE('',#6683,1.4);
#6039=CYLINDRICAL_SURFACE('',#6693,0.3);
#6040=CYLINDRICAL_SURFACE('',#6700,0.4);
#6041=CYLINDRICAL_SURFACE('',#6705,0.6);
#6042=CYLINDRICAL_SURFACE('',#6708,0.4);
#6043=CYLINDRICAL_SURFACE('',#6716,0.3);
#6044=CYLINDRICAL_SURFACE('',#6718,0.6);
#6045=CYLINDRICAL_SURFACE('',#6723,0.25);
#6046=CYLINDRICAL_SURFACE('',#6725,0.25);
#6047=CYLINDRICAL_SURFACE('',#6727,0.25);
#6048=CYLINDRICAL_SURFACE('',#6729,0.25);
#6049=CYLINDRICAL_SURFACE('',#6735,0.15);
#6050=CYLINDRICAL_SURFACE('',#6737,0.15);
#6051=CYLINDRICAL_SURFACE('',#6740,0.15);
#6052=CYLINDRICAL_SURFACE('',#6743,0.15);
#6053=CYLINDRICAL_SURFACE('',#6745,0.3);
#6054=CYLINDRICAL_SURFACE('',#6750,0.3);
#6055=CYLINDRICAL_SURFACE('',#6755,0.17);
#6056=CYLINDRICAL_SURFACE('',#6757,0.17);
#6057=CYLINDRICAL_SURFACE('',#6781,0.4);
#6058=CYLINDRICAL_SURFACE('',#6782,0.4);
#6059=CYLINDRICAL_SURFACE('',#6805,0.1);
#6060=CYLINDRICAL_SURFACE('',#6809,0.1);
#6061=CYLINDRICAL_SURFACE('',#6823,0.3);
#6062=CYLINDRICAL_SURFACE('',#6828,0.3);
#6063=CYLINDRICAL_SURFACE('',#6833,0.25);
#6064=CYLINDRICAL_SURFACE('',#6835,0.25);
#6065=CYLINDRICAL_SURFACE('',#6837,0.25);
#6066=CYLINDRICAL_SURFACE('',#6839,0.25);
#6067=CYLINDRICAL_SURFACE('',#6861,0.15);
#6068=CYLINDRICAL_SURFACE('',#6863,0.15);
#6069=CYLINDRICAL_SURFACE('',#6866,0.15);
#6070=CYLINDRICAL_SURFACE('',#6869,0.15);
#6071=CYLINDRICAL_SURFACE('',#6871,0.17);
#6072=CYLINDRICAL_SURFACE('',#6873,0.17);
#6073=CYLINDRICAL_SURFACE('',#6897,0.4);
#6074=CYLINDRICAL_SURFACE('',#6898,0.4);
#6075=CYLINDRICAL_SURFACE('',#6921,0.1);
#6076=CYLINDRICAL_SURFACE('',#6925,0.1);
#6077=CYLINDRICAL_SURFACE('',#6939,0.3);
#6078=CYLINDRICAL_SURFACE('',#6944,0.3);
#6079=CYLINDRICAL_SURFACE('',#6949,0.14635);
#6080=CYLINDRICAL_SURFACE('',#6951,0.14635);
#6081=CYLINDRICAL_SURFACE('',#6952,0.14635);
#6082=CYLINDRICAL_SURFACE('',#6953,0.14635);
#6083=CYLINDRICAL_SURFACE('',#6954,0.14635);
#6084=CYLINDRICAL_SURFACE('',#6955,0.14635);
#6085=CYLINDRICAL_SURFACE('',#6956,0.14635);
#6086=CYLINDRICAL_SURFACE('',#6957,0.14635);
#6087=CYLINDRICAL_SURFACE('',#6958,0.14635);
#6088=CYLINDRICAL_SURFACE('',#6959,0.14635);
#6089=CYLINDRICAL_SURFACE('',#6960,0.14635);
#6090=CYLINDRICAL_SURFACE('',#6961,0.14635);
#6091=CYLINDRICAL_SURFACE('',#6962,0.14635);
#6092=CYLINDRICAL_SURFACE('',#6963,0.14635);
#6093=CYLINDRICAL_SURFACE('',#6964,0.14635);
#6094=CYLINDRICAL_SURFACE('',#6965,0.14635);
#6095=CYLINDRICAL_SURFACE('',#6966,0.14635);
#6096=CYLINDRICAL_SURFACE('',#6967,0.14635);
#6097=CYLINDRICAL_SURFACE('',#6968,0.14635);
#6098=CYLINDRICAL_SURFACE('',#6969,0.14635);
#6099=CYLINDRICAL_SURFACE('',#6970,0.14635);
#6100=CYLINDRICAL_SURFACE('',#6971,0.14635);
#6101=CYLINDRICAL_SURFACE('',#6972,0.14635);
#6102=CYLINDRICAL_SURFACE('',#6973,0.14635);
#6103=CYLINDRICAL_SURFACE('',#6974,0.14635);
#6104=CYLINDRICAL_SURFACE('',#6975,0.14635);
#6105=CYLINDRICAL_SURFACE('',#6976,0.14635);
#6106=CYLINDRICAL_SURFACE('',#6977,0.14635);
#6107=CYLINDRICAL_SURFACE('',#6978,0.14635);
#6108=CYLINDRICAL_SURFACE('',#6979,0.14635);
#6109=CYLINDRICAL_SURFACE('',#6980,0.117775);
#6110=CYLINDRICAL_SURFACE('',#6982,0.117775);
#6111=CYLINDRICAL_SURFACE('',#6983,0.117775);
#6112=CYLINDRICAL_SURFACE('',#6984,0.117775);
#6113=CYLINDRICAL_SURFACE('',#6985,0.117775);
#6114=CYLINDRICAL_SURFACE('',#6986,0.117775);
#6115=CYLINDRICAL_SURFACE('',#6987,0.117775);
#6116=CYLINDRICAL_SURFACE('',#6988,0.117775);
#6117=CYLINDRICAL_SURFACE('',#6989,0.117775);
#6118=CYLINDRICAL_SURFACE('',#6990,0.117775);
#6119=CYLINDRICAL_SURFACE('',#6991,0.117775);
#6120=CYLINDRICAL_SURFACE('',#6992,0.117775);
#6121=CYLINDRICAL_SURFACE('',#6993,0.117775);
#6122=CYLINDRICAL_SURFACE('',#6994,0.117775);
#6123=CYLINDRICAL_SURFACE('',#6995,0.117775);
#6124=CYLINDRICAL_SURFACE('',#6996,0.117775);
#6125=CYLINDRICAL_SURFACE('',#6997,0.117775);
#6126=CYLINDRICAL_SURFACE('',#6998,0.117775);
#6127=CYLINDRICAL_SURFACE('',#6999,0.117775);
#6128=CYLINDRICAL_SURFACE('',#7000,0.117775);
#6129=CYLINDRICAL_SURFACE('',#7001,0.117775);
#6130=CYLINDRICAL_SURFACE('',#7002,0.117775);
#6131=CYLINDRICAL_SURFACE('',#7003,0.117775);
#6132=CYLINDRICAL_SURFACE('',#7004,0.117775);
#6133=CYLINDRICAL_SURFACE('',#7005,0.117775);
#6134=CYLINDRICAL_SURFACE('',#7006,0.117775);
#6135=CYLINDRICAL_SURFACE('',#7007,0.117775);
#6136=CYLINDRICAL_SURFACE('',#7008,0.117775);
#6137=CYLINDRICAL_SURFACE('',#7009,0.117775);
#6138=CYLINDRICAL_SURFACE('',#7010,0.117775);
#6139=CYLINDRICAL_SURFACE('',#7014,0.117775);
#6140=CYLINDRICAL_SURFACE('',#7016,0.14635);
#6141=CYLINDRICAL_SURFACE('',#7026,0.275);
#6142=CYLINDRICAL_SURFACE('',#7031,0.12645);
#6143=CYLINDRICAL_SURFACE('',#7033,0.12645);
#6144=CYLINDRICAL_SURFACE('',#7035,0.12645);
#6145=CYLINDRICAL_SURFACE('',#7036,0.12645);
#6146=CYLINDRICAL_SURFACE('',#7037,0.12645);
#6147=CYLINDRICAL_SURFACE('',#7039,0.1543);
#6148=CYLINDRICAL_SURFACE('',#7041,0.1543);
#6149=CYLINDRICAL_SURFACE('',#7042,0.1543);
#6150=CYLINDRICAL_SURFACE('',#7043,0.1543);
#6151=CYLINDRICAL_SURFACE('',#7044,0.1543);
#6152=CYLINDRICAL_SURFACE('',#7046,0.1543);
#6153=CYLINDRICAL_SURFACE('',#7048,0.12645);
#6154=CYLINDRICAL_SURFACE('',#7057,0.35);
#6155=CYLINDRICAL_SURFACE('',#7060,0.35);
#6156=CYLINDRICAL_SURFACE('',#7066,0.25);
#6157=CYLINDRICAL_SURFACE('',#7072,0.25);
#6158=CYLINDRICAL_SURFACE('',#7078,0.25);
#6159=CYLINDRICAL_SURFACE('',#7084,0.25);
#6160=CYLINDRICAL_SURFACE('',#7087,0.15);
#6161=CYLINDRICAL_SURFACE('',#7089,0.15);
#6162=CYLINDRICAL_SURFACE('',#7091,0.15);
#6163=CYLINDRICAL_SURFACE('',#7093,0.15);
#6164=CYLINDRICAL_SURFACE('',#7097,0.08);
#6165=CYLINDRICAL_SURFACE('',#7102,0.08);
#6166=CYLINDRICAL_SURFACE('',#7118,0.41);
#6167=CYLINDRICAL_SURFACE('',#7121,0.6);
#6168=ADVANCED_FACE('',(#796),#6034,.F.);
#6169=ADVANCED_FACE('',(#797),#6035,.F.);
#6170=ADVANCED_FACE('',(#798),#6036,.F.);
#6171=ADVANCED_FACE('',(#799),#651,.F.);
#6172=ADVANCED_FACE('',(#800),#652,.F.);
#6173=ADVANCED_FACE('',(#801),#653,.T.);
#6174=ADVANCED_FACE('',(#802),#654,.T.);
#6175=ADVANCED_FACE('',(#803),#655,.T.);
#6176=ADVANCED_FACE('',(#804),#656,.T.);
#6177=ADVANCED_FACE('',(#805),#657,.T.);
#6178=ADVANCED_FACE('',(#806),#658,.T.);
#6179=ADVANCED_FACE('',(#807),#659,.T.);
#6180=ADVANCED_FACE('',(#808),#660,.T.);
#6181=ADVANCED_FACE('',(#809,#590,#591,#592),#661,.F.);
#6182=ADVANCED_FACE('',(#810),#662,.T.);
#6183=ADVANCED_FACE('',(#811),#663,.T.);
#6184=ADVANCED_FACE('',(#812),#664,.T.);
#6185=ADVANCED_FACE('',(#813),#665,.T.);
#6186=ADVANCED_FACE('',(#814),#6037,.T.);
#6187=ADVANCED_FACE('',(#815),#6038,.T.);
#6188=ADVANCED_FACE('',(#816,#593,#594,#595),#666,.T.);
#6189=ADVANCED_FACE('',(#817),#667,.T.);
#6190=ADVANCED_FACE('',(#818),#668,.T.);
#6191=ADVANCED_FACE('',(#819),#669,.T.);
#6192=ADVANCED_FACE('',(#820),#670,.T.);
#6193=ADVANCED_FACE('',(#821),#671,.T.);
#6194=ADVANCED_FACE('',(#822),#672,.T.);
#6195=ADVANCED_FACE('',(#823),#6039,.T.);
#6196=ADVANCED_FACE('',(#824,#596),#673,.F.);
#6197=ADVANCED_FACE('',(#825,#597),#674,.F.);
#6198=ADVANCED_FACE('',(#826),#6040,.T.);
#6199=ADVANCED_FACE('',(#827,#598),#675,.T.);
#6200=ADVANCED_FACE('',(#828),#6041,.T.);
#6201=ADVANCED_FACE('',(#829),#676,.F.);
#6202=ADVANCED_FACE('',(#830),#6042,.T.);
#6203=ADVANCED_FACE('',(#831),#677,.T.);
#6204=ADVANCED_FACE('',(#832),#678,.F.);
#6205=ADVANCED_FACE('',(#833),#679,.F.);
#6206=ADVANCED_FACE('',(#834),#680,.F.);
#6207=ADVANCED_FACE('',(#835),#6043,.F.);
#6208=ADVANCED_FACE('',(#836),#6044,.T.);
#6209=ADVANCED_FACE('',(#837),#681,.T.);
#6210=ADVANCED_FACE('',(#838),#6045,.F.);
#6211=ADVANCED_FACE('',(#839),#6046,.F.);
#6212=ADVANCED_FACE('',(#840),#6047,.F.);
#6213=ADVANCED_FACE('',(#841),#6048,.F.);
#6214=ADVANCED_FACE('',(#842),#92,.T.);
#6215=ADVANCED_FACE('',(#843),#93,.T.);
#6216=ADVANCED_FACE('',(#844,#599,#600,#601),#682,.F.);
#6217=ADVANCED_FACE('',(#845),#6049,.F.);
#6218=ADVANCED_FACE('',(#846),#6050,.F.);
#6219=ADVANCED_FACE('',(#847),#6051,.F.);
#6220=ADVANCED_FACE('',(#848),#6052,.F.);
#6221=ADVANCED_FACE('',(#849),#6053,.F.);
#6222=ADVANCED_FACE('',(#850,#602),#683,.F.);
#6223=ADVANCED_FACE('',(#851),#6054,.F.);
#6224=ADVANCED_FACE('',(#852,#603),#684,.F.);
#6225=ADVANCED_FACE('',(#853),#6055,.F.);
#6226=ADVANCED_FACE('',(#854),#6056,.F.);
#6227=ADVANCED_FACE('',(#855),#685,.F.);
#6228=ADVANCED_FACE('',(#856),#686,.F.);
#6229=ADVANCED_FACE('',(#857),#687,.F.);
#6230=ADVANCED_FACE('',(#858),#688,.F.);
#6231=ADVANCED_FACE('',(#859),#689,.F.);
#6232=ADVANCED_FACE('',(#860),#690,.F.);
#6233=ADVANCED_FACE('',(#861),#691,.F.);
#6234=ADVANCED_FACE('',(#862,#604),#692,.F.);
#6235=ADVANCED_FACE('',(#863,#605),#693,.F.);
#6236=ADVANCED_FACE('',(#864),#694,.F.);
#6237=ADVANCED_FACE('',(#865),#695,.F.);
#6238=ADVANCED_FACE('',(#866),#696,.F.);
#6239=ADVANCED_FACE('',(#867),#697,.F.);
#6240=ADVANCED_FACE('',(#868),#698,.F.);
#6241=ADVANCED_FACE('',(#869),#699,.T.);
#6242=ADVANCED_FACE('',(#870),#700,.T.);
#6243=ADVANCED_FACE('',(#871),#701,.T.);
#6244=ADVANCED_FACE('',(#872),#702,.T.);
#6245=ADVANCED_FACE('',(#873),#703,.T.);
#6246=ADVANCED_FACE('',(#874,#606),#704,.F.);
#6247=ADVANCED_FACE('',(#875),#6057,.T.);
#6248=ADVANCED_FACE('',(#876),#6058,.T.);
#6249=ADVANCED_FACE('',(#877),#705,.T.);
#6250=ADVANCED_FACE('',(#878),#94,.T.);
#6251=ADVANCED_FACE('',(#879),#95,.T.);
#6252=ADVANCED_FACE('',(#880),#96,.T.);
#6253=ADVANCED_FACE('',(#881),#97,.T.);
#6254=ADVANCED_FACE('',(#882),#706,.F.);
#6255=ADVANCED_FACE('',(#883),#98,.T.);
#6256=ADVANCED_FACE('',(#884),#99,.T.);
#6257=ADVANCED_FACE('',(#885),#707,.T.);
#6258=ADVANCED_FACE('',(#886),#100,.T.);
#6259=ADVANCED_FACE('',(#887),#101,.T.);
#6260=ADVANCED_FACE('',(#888),#708,.F.);
#6261=ADVANCED_FACE('',(#889),#102,.T.);
#6262=ADVANCED_FACE('',(#890),#103,.T.);
#6263=ADVANCED_FACE('',(#891),#709,.T.);
#6264=ADVANCED_FACE('',(#892),#104,.T.);
#6265=ADVANCED_FACE('',(#893),#105,.T.);
#6266=ADVANCED_FACE('',(#894,#607,#608,#609),#710,.F.);
#6267=ADVANCED_FACE('',(#895),#106,.T.);
#6268=ADVANCED_FACE('',(#896),#711,.T.);
#6269=ADVANCED_FACE('',(#897),#107,.T.);
#6270=ADVANCED_FACE('',(#898),#108,.T.);
#6271=ADVANCED_FACE('',(#899),#712,.F.);
#6272=ADVANCED_FACE('',(#900),#109,.T.);
#6273=ADVANCED_FACE('',(#901),#110,.T.);
#6274=ADVANCED_FACE('',(#902),#76,.F.);
#6275=ADVANCED_FACE('',(#903),#77,.F.);
#6276=ADVANCED_FACE('',(#904),#78,.F.);
#6277=ADVANCED_FACE('',(#905),#6059,.F.);
#6278=ADVANCED_FACE('',(#906),#111,.T.);
#6279=ADVANCED_FACE('',(#907),#79,.F.);
#6280=ADVANCED_FACE('',(#908),#6060,.F.);
#6281=ADVANCED_FACE('',(#909),#112,.T.);
#6282=ADVANCED_FACE('',(#910),#113,.T.);
#6283=ADVANCED_FACE('',(#911),#114,.T.);
#6284=ADVANCED_FACE('',(#912),#115,.T.);
#6285=ADVANCED_FACE('',(#913),#713,.T.);
#6286=ADVANCED_FACE('',(#914),#80,.T.);
#6287=ADVANCED_FACE('',(#915),#81,.T.);
#6288=ADVANCED_FACE('',(#916),#82,.T.);
#6289=ADVANCED_FACE('',(#917),#6061,.T.);
#6290=ADVANCED_FACE('',(#918),#116,.F.);
#6291=ADVANCED_FACE('',(#919),#83,.T.);
#6292=ADVANCED_FACE('',(#920),#6062,.T.);
#6293=ADVANCED_FACE('',(#921),#117,.F.);
#6294=ADVANCED_FACE('',(#922),#118,.F.);
#6295=ADVANCED_FACE('',(#923),#119,.F.);
#6296=ADVANCED_FACE('',(#924),#120,.F.);
#6297=ADVANCED_FACE('',(#925),#121,.F.);
#6298=ADVANCED_FACE('',(#926),#122,.F.);
#6299=ADVANCED_FACE('',(#927),#714,.F.);
#6300=ADVANCED_FACE('',(#928,#610,#611,#612,#613,#614,#615),#715,.T.);
#6301=ADVANCED_FACE('',(#929),#123,.F.);
#6302=ADVANCED_FACE('',(#930),#716,.F.);
#6303=ADVANCED_FACE('',(#931),#6063,.F.);
#6304=ADVANCED_FACE('',(#932),#6064,.F.);
#6305=ADVANCED_FACE('',(#933),#6065,.F.);
#6306=ADVANCED_FACE('',(#934),#6066,.F.);
#6307=ADVANCED_FACE('',(#935),#124,.T.);
#6308=ADVANCED_FACE('',(#936),#125,.T.);
#6309=ADVANCED_FACE('',(#937,#616,#617,#618),#717,.F.);
#6310=ADVANCED_FACE('',(#938),#718,.F.);
#6311=ADVANCED_FACE('',(#939),#719,.F.);
#6312=ADVANCED_FACE('',(#940),#720,.F.);
#6313=ADVANCED_FACE('',(#941),#721,.F.);
#6314=ADVANCED_FACE('',(#942),#722,.F.);
#6315=ADVANCED_FACE('',(#943),#723,.F.);
#6316=ADVANCED_FACE('',(#944,#619),#724,.F.);
#6317=ADVANCED_FACE('',(#945),#725,.F.);
#6318=ADVANCED_FACE('',(#946),#726,.F.);
#6319=ADVANCED_FACE('',(#947),#727,.F.);
#6320=ADVANCED_FACE('',(#948),#728,.F.);
#6321=ADVANCED_FACE('',(#949),#729,.F.);
#6322=ADVANCED_FACE('',(#950),#730,.F.);
#6323=ADVANCED_FACE('',(#951,#620),#731,.F.);
#6324=ADVANCED_FACE('',(#952),#6067,.F.);
#6325=ADVANCED_FACE('',(#953),#6068,.F.);
#6326=ADVANCED_FACE('',(#954),#6069,.F.);
#6327=ADVANCED_FACE('',(#955),#6070,.F.);
#6328=ADVANCED_FACE('',(#956),#6071,.F.);
#6329=ADVANCED_FACE('',(#957),#6072,.F.);
#6330=ADVANCED_FACE('',(#958),#732,.F.);
#6331=ADVANCED_FACE('',(#959),#733,.F.);
#6332=ADVANCED_FACE('',(#960),#734,.F.);
#6333=ADVANCED_FACE('',(#961),#735,.F.);
#6334=ADVANCED_FACE('',(#962),#736,.F.);
#6335=ADVANCED_FACE('',(#963),#737,.F.);
#6336=ADVANCED_FACE('',(#964),#738,.F.);
#6337=ADVANCED_FACE('',(#965,#621),#739,.F.);
#6338=ADVANCED_FACE('',(#966,#622),#740,.F.);
#6339=ADVANCED_FACE('',(#967),#741,.F.);
#6340=ADVANCED_FACE('',(#968),#742,.F.);
#6341=ADVANCED_FACE('',(#969),#743,.F.);
#6342=ADVANCED_FACE('',(#970),#744,.F.);
#6343=ADVANCED_FACE('',(#971),#745,.F.);
#6344=ADVANCED_FACE('',(#972),#746,.T.);
#6345=ADVANCED_FACE('',(#973),#747,.T.);
#6346=ADVANCED_FACE('',(#974),#748,.T.);
#6347=ADVANCED_FACE('',(#975),#749,.T.);
#6348=ADVANCED_FACE('',(#976),#750,.T.);
#6349=ADVANCED_FACE('',(#977,#623),#751,.F.);
#6350=ADVANCED_FACE('',(#978),#6073,.T.);
#6351=ADVANCED_FACE('',(#979),#6074,.T.);
#6352=ADVANCED_FACE('',(#980),#752,.T.);
#6353=ADVANCED_FACE('',(#981),#126,.T.);
#6354=ADVANCED_FACE('',(#982),#127,.T.);
#6355=ADVANCED_FACE('',(#983),#128,.T.);
#6356=ADVANCED_FACE('',(#984),#129,.T.);
#6357=ADVANCED_FACE('',(#985),#753,.F.);
#6358=ADVANCED_FACE('',(#986),#130,.T.);
#6359=ADVANCED_FACE('',(#987),#131,.T.);
#6360=ADVANCED_FACE('',(#988),#754,.T.);
#6361=ADVANCED_FACE('',(#989),#132,.T.);
#6362=ADVANCED_FACE('',(#990),#133,.T.);
#6363=ADVANCED_FACE('',(#991),#755,.F.);
#6364=ADVANCED_FACE('',(#992),#134,.T.);
#6365=ADVANCED_FACE('',(#993),#135,.T.);
#6366=ADVANCED_FACE('',(#994),#756,.T.);
#6367=ADVANCED_FACE('',(#995),#136,.T.);
#6368=ADVANCED_FACE('',(#996),#137,.T.);
#6369=ADVANCED_FACE('',(#997,#624,#625,#626),#757,.F.);
#6370=ADVANCED_FACE('',(#998),#138,.T.);
#6371=ADVANCED_FACE('',(#999),#758,.T.);
#6372=ADVANCED_FACE('',(#1000),#139,.T.);
#6373=ADVANCED_FACE('',(#1001),#140,.T.);
#6374=ADVANCED_FACE('',(#1002),#759,.F.);
#6375=ADVANCED_FACE('',(#1003),#141,.T.);
#6376=ADVANCED_FACE('',(#1004),#142,.T.);
#6377=ADVANCED_FACE('',(#1005),#84,.F.);
#6378=ADVANCED_FACE('',(#1006),#85,.F.);
#6379=ADVANCED_FACE('',(#1007),#86,.F.);
#6380=ADVANCED_FACE('',(#1008),#6075,.F.);
#6381=ADVANCED_FACE('',(#1009),#143,.T.);
#6382=ADVANCED_FACE('',(#1010),#87,.F.);
#6383=ADVANCED_FACE('',(#1011),#6076,.F.);
#6384=ADVANCED_FACE('',(#1012),#144,.T.);
#6385=ADVANCED_FACE('',(#1013),#145,.T.);
#6386=ADVANCED_FACE('',(#1014),#146,.T.);
#6387=ADVANCED_FACE('',(#1015),#147,.T.);
#6388=ADVANCED_FACE('',(#1016),#760,.T.);
#6389=ADVANCED_FACE('',(#1017),#88,.T.);
#6390=ADVANCED_FACE('',(#1018),#89,.T.);
#6391=ADVANCED_FACE('',(#1019),#90,.T.);
#6392=ADVANCED_FACE('',(#1020),#6077,.T.);
#6393=ADVANCED_FACE('',(#1021),#148,.F.);
#6394=ADVANCED_FACE('',(#1022),#91,.T.);
#6395=ADVANCED_FACE('',(#1023),#6078,.T.);
#6396=ADVANCED_FACE('',(#1024),#149,.F.);
#6397=ADVANCED_FACE('',(#1025),#150,.F.);
#6398=ADVANCED_FACE('',(#1026),#151,.F.);
#6399=ADVANCED_FACE('',(#1027),#152,.F.);
#6400=ADVANCED_FACE('',(#1028),#153,.F.);
#6401=ADVANCED_FACE('',(#1029),#154,.F.);
#6402=ADVANCED_FACE('',(#1030),#761,.F.);
#6403=ADVANCED_FACE('',(#1031,#627,#628,#629,#630,#631,#632),#762,.T.);
#6404=ADVANCED_FACE('',(#1032),#155,.F.);
#6405=ADVANCED_FACE('',(#1033),#763,.F.);
#6406=ADVANCED_FACE('',(#1034),#6079,.T.);
#6407=ADVANCED_FACE('',(#1035),#6080,.T.);
#6408=ADVANCED_FACE('',(#1036),#6081,.T.);
#6409=ADVANCED_FACE('',(#1037),#6082,.T.);
#6410=ADVANCED_FACE('',(#1038),#6083,.T.);
#6411=ADVANCED_FACE('',(#1039),#6084,.T.);
#6412=ADVANCED_FACE('',(#1040),#6085,.T.);
#6413=ADVANCED_FACE('',(#1041),#6086,.T.);
#6414=ADVANCED_FACE('',(#1042),#6087,.T.);
#6415=ADVANCED_FACE('',(#1043),#6088,.T.);
#6416=ADVANCED_FACE('',(#1044),#6089,.T.);
#6417=ADVANCED_FACE('',(#1045),#6090,.T.);
#6418=ADVANCED_FACE('',(#1046),#6091,.T.);
#6419=ADVANCED_FACE('',(#1047),#6092,.T.);
#6420=ADVANCED_FACE('',(#1048),#6093,.T.);
#6421=ADVANCED_FACE('',(#1049),#6094,.T.);
#6422=ADVANCED_FACE('',(#1050),#6095,.T.);
#6423=ADVANCED_FACE('',(#1051),#6096,.T.);
#6424=ADVANCED_FACE('',(#1052),#6097,.T.);
#6425=ADVANCED_FACE('',(#1053),#6098,.T.);
#6426=ADVANCED_FACE('',(#1054),#6099,.T.);
#6427=ADVANCED_FACE('',(#1055),#6100,.T.);
#6428=ADVANCED_FACE('',(#1056),#6101,.T.);
#6429=ADVANCED_FACE('',(#1057),#6102,.T.);
#6430=ADVANCED_FACE('',(#1058),#6103,.T.);
#6431=ADVANCED_FACE('',(#1059),#6104,.T.);
#6432=ADVANCED_FACE('',(#1060),#6105,.T.);
#6433=ADVANCED_FACE('',(#1061),#6106,.T.);
#6434=ADVANCED_FACE('',(#1062),#6107,.T.);
#6435=ADVANCED_FACE('',(#1063),#6108,.T.);
#6436=ADVANCED_FACE('',(#1064),#6109,.T.);
#6437=ADVANCED_FACE('',(#1065),#6110,.T.);
#6438=ADVANCED_FACE('',(#1066),#6111,.T.);
#6439=ADVANCED_FACE('',(#1067),#6112,.T.);
#6440=ADVANCED_FACE('',(#1068),#6113,.T.);
#6441=ADVANCED_FACE('',(#1069),#6114,.T.);
#6442=ADVANCED_FACE('',(#1070),#6115,.T.);
#6443=ADVANCED_FACE('',(#1071),#6116,.T.);
#6444=ADVANCED_FACE('',(#1072),#6117,.T.);
#6445=ADVANCED_FACE('',(#1073),#6118,.T.);
#6446=ADVANCED_FACE('',(#1074),#6119,.T.);
#6447=ADVANCED_FACE('',(#1075),#6120,.T.);
#6448=ADVANCED_FACE('',(#1076),#6121,.T.);
#6449=ADVANCED_FACE('',(#1077),#6122,.T.);
#6450=ADVANCED_FACE('',(#1078),#6123,.T.);
#6451=ADVANCED_FACE('',(#1079),#6124,.T.);
#6452=ADVANCED_FACE('',(#1080),#6125,.T.);
#6453=ADVANCED_FACE('',(#1081),#6126,.T.);
#6454=ADVANCED_FACE('',(#1082),#6127,.T.);
#6455=ADVANCED_FACE('',(#1083),#6128,.T.);
#6456=ADVANCED_FACE('',(#1084),#6129,.T.);
#6457=ADVANCED_FACE('',(#1085),#6130,.T.);
#6458=ADVANCED_FACE('',(#1086),#6131,.T.);
#6459=ADVANCED_FACE('',(#1087),#6132,.T.);
#6460=ADVANCED_FACE('',(#1088),#6133,.T.);
#6461=ADVANCED_FACE('',(#1089),#6134,.T.);
#6462=ADVANCED_FACE('',(#1090),#6135,.T.);
#6463=ADVANCED_FACE('',(#1091),#6136,.T.);
#6464=ADVANCED_FACE('',(#1092),#6137,.T.);
#6465=ADVANCED_FACE('',(#1093),#6138,.T.);
#6466=ADVANCED_FACE('',(#1094),#75,.T.);
#6467=ADVANCED_FACE('',(#1095),#156,.F.);
#6468=ADVANCED_FACE('',(#1096),#6139,.T.);
#6469=ADVANCED_FACE('',(#1097),#157,.F.);
#6470=ADVANCED_FACE('',(#1098),#6140,.T.);
#6471=ADVANCED_FACE('',(#1099),#764,.F.);
#6472=ADVANCED_FACE('',(#1100),#765,.F.);
#6473=ADVANCED_FACE('',(#1101),#766,.F.);
#6474=ADVANCED_FACE('',(#1102),#767,.F.);
#6475=ADVANCED_FACE('',(#1103),#768,.F.);
#6476=ADVANCED_FACE('',(#1104),#769,.F.);
#6477=ADVANCED_FACE('',(#1105),#770,.F.);
#6478=ADVANCED_FACE('',(#1106,#633),#771,.T.);
#6479=ADVANCED_FACE('',(#1107),#6141,.T.);
#6480=ADVANCED_FACE('',(#1108,#634),#772,.F.);
#6481=ADVANCED_FACE('',(#1109),#773,.T.);
#6482=ADVANCED_FACE('',(#1110),#6142,.F.);
#6483=ADVANCED_FACE('',(#1111),#6143,.F.);
#6484=ADVANCED_FACE('',(#1112),#6144,.F.);
#6485=ADVANCED_FACE('',(#1113),#6145,.F.);
#6486=ADVANCED_FACE('',(#1114),#6146,.F.);
#6487=ADVANCED_FACE('',(#1115),#6147,.F.);
#6488=ADVANCED_FACE('',(#1116),#6148,.F.);
#6489=ADVANCED_FACE('',(#1117),#6149,.F.);
#6490=ADVANCED_FACE('',(#1118),#6150,.F.);
#6491=ADVANCED_FACE('',(#1119),#6151,.F.);
#6492=ADVANCED_FACE('',(#1120),#6152,.F.);
#6493=ADVANCED_FACE('',(#1121),#158,.F.);
#6494=ADVANCED_FACE('',(#1122),#159,.F.);
#6495=ADVANCED_FACE('',(#1123,#635),#774,.T.);
#6496=ADVANCED_FACE('',(#1124),#6153,.F.);
#6497=ADVANCED_FACE('',(#1125),#775,.T.);
#6498=ADVANCED_FACE('',(#1126),#776,.T.);
#6499=ADVANCED_FACE('',(#1127),#777,.T.);
#6500=ADVANCED_FACE('',(#1128),#778,.T.);
#6501=ADVANCED_FACE('',(#1129),#779,.T.);
#6502=ADVANCED_FACE('',(#1130),#780,.T.);
#6503=ADVANCED_FACE('',(#1131,#636),#781,.F.);
#6504=ADVANCED_FACE('',(#1132),#6154,.F.);
#6505=ADVANCED_FACE('',(#1133),#6155,.F.);
#6506=ADVANCED_FACE('',(#1134,#637),#782,.T.);
#6507=ADVANCED_FACE('',(#1135),#6156,.T.);
#6508=ADVANCED_FACE('',(#1136),#783,.F.);
#6509=ADVANCED_FACE('',(#1137,#638),#784,.T.);
#6510=ADVANCED_FACE('',(#1138),#6157,.T.);
#6511=ADVANCED_FACE('',(#1139),#785,.F.);
#6512=ADVANCED_FACE('',(#1140,#639),#786,.T.);
#6513=ADVANCED_FACE('',(#1141),#6158,.T.);
#6514=ADVANCED_FACE('',(#1142),#787,.F.);
#6515=ADVANCED_FACE('',(#1143,#640),#788,.T.);
#6516=ADVANCED_FACE('',(#1144),#6159,.T.);
#6517=ADVANCED_FACE('',(#1145),#789,.F.);
#6518=ADVANCED_FACE('',(#1146),#6160,.T.);
#6519=ADVANCED_FACE('',(#1147),#6161,.T.);
#6520=ADVANCED_FACE('',(#1148),#6162,.T.);
#6521=ADVANCED_FACE('',(#1149),#6163,.T.);
#6522=ADVANCED_FACE('',(#1150),#160,.F.);
#6523=ADVANCED_FACE('',(#1151),#6164,.T.);
#6524=ADVANCED_FACE('',(#1152),#161,.F.);
#6525=ADVANCED_FACE('',(#1153),#162,.F.);
#6526=ADVANCED_FACE('',(#1154),#163,.F.);
#6527=ADVANCED_FACE('',(#1155),#6165,.T.);
#6528=ADVANCED_FACE('',(#1156),#164,.F.);
#6529=ADVANCED_FACE('',(#1157),#165,.F.);
#6530=ADVANCED_FACE('',(#1158),#790,.F.);
#6531=ADVANCED_FACE('',(#1159),#166,.F.);
#6532=ADVANCED_FACE('',(#1160),#167,.F.);
#6533=ADVANCED_FACE('',(#1161),#168,.F.);
#6534=ADVANCED_FACE('',(#1162,#641,#642),#791,.T.);
#6535=ADVANCED_FACE('',(#1163),#792,.F.);
#6536=ADVANCED_FACE('',(#1164),#169,.F.);
#6537=ADVANCED_FACE('',(#1165),#170,.F.);
#6538=ADVANCED_FACE('',(#1166,#643,#644,#645,#646,#647,#648),#793,.F.);
#6539=ADVANCED_FACE('',(#1167),#171,.F.);
#6540=ADVANCED_FACE('',(#1168),#6166,.F.);
#6541=ADVANCED_FACE('',(#1169),#6167,.T.);
#6542=ADVANCED_FACE('',(#1170,#649),#794,.T.);
#6543=ADVANCED_FACE('',(#1171,#650),#795,.F.);
#6544=CLOSED_SHELL('',(#6168,#6169,#6170,#6171,#6172,#6173,#6174,#6175,
#6176,#6177,#6178,#6179,#6180,#6181,#6182,#6183,#6184,#6185,#6186,#6187,
#6188,#6189,#6190,#6191,#6192,#6193,#6194));
#6545=CLOSED_SHELL('',(#6195,#6196,#6197,#6198,#6199,#6200,#6201,#6202,
#6203));
#6546=CLOSED_SHELL('',(#6204,#6205,#6206,#6207,#6208,#6209));
#6547=CLOSED_SHELL('',(#6210,#6211,#6212,#6213,#6214,#6215,#6216,#6217,
#6218,#6219,#6220,#6221,#6222,#6223,#6224,#6225,#6226,#6227,#6228,#6229,
#6230,#6231,#6232,#6233,#6234,#6235,#6236,#6237,#6238,#6239,#6240,#6241,
#6242,#6243,#6244,#6245,#6246,#6247,#6248,#6249,#6250,#6251,#6252,#6253,
#6254,#6255,#6256,#6257,#6258,#6259,#6260,#6261,#6262,#6263,#6264,#6265,
#6266,#6267,#6268,#6269,#6270,#6271,#6272,#6273,#6274,#6275,#6276,#6277,
#6278,#6279,#6280,#6281,#6282,#6283,#6284,#6285,#6286,#6287,#6288,#6289,
#6290,#6291,#6292,#6293,#6294,#6295,#6296,#6297,#6298,#6299,#6300,#6301,
#6302));
#6548=CLOSED_SHELL('',(#6303,#6304,#6305,#6306,#6307,#6308,#6309,#6310,
#6311,#6312,#6313,#6314,#6315,#6316,#6317,#6318,#6319,#6320,#6321,#6322,
#6323,#6324,#6325,#6326,#6327,#6328,#6329,#6330,#6331,#6332,#6333,#6334,
#6335,#6336,#6337,#6338,#6339,#6340,#6341,#6342,#6343,#6344,#6345,#6346,
#6347,#6348,#6349,#6350,#6351,#6352,#6353,#6354,#6355,#6356,#6357,#6358,
#6359,#6360,#6361,#6362,#6363,#6364,#6365,#6366,#6367,#6368,#6369,#6370,
#6371,#6372,#6373,#6374,#6375,#6376,#6377,#6378,#6379,#6380,#6381,#6382,
#6383,#6384,#6385,#6386,#6387,#6388,#6389,#6390,#6391,#6392,#6393,#6394,
#6395,#6396,#6397,#6398,#6399,#6400,#6401,#6402,#6403,#6404,#6405));
#6549=CLOSED_SHELL('',(#6406,#6407,#6408,#6409,#6410,#6411,#6412,#6413,
#6414,#6415,#6416,#6417,#6418,#6419,#6420,#6421,#6422,#6423,#6424,#6425,
#6426,#6427,#6428,#6429,#6430,#6431,#6432,#6433,#6434,#6435,#6436,#6437,
#6438,#6439,#6440,#6441,#6442,#6443,#6444,#6445,#6446,#6447,#6448,#6449,
#6450,#6451,#6452,#6453,#6454,#6455,#6456,#6457,#6458,#6459,#6460,#6461,
#6462,#6463,#6464,#6465,#6466,#6467,#6468,#6469,#6470,#6471,#6472,#6473,
#6474,#6475,#6476,#6477,#6478,#6479,#6480,#6481));
#6550=CLOSED_SHELL('',(#6482,#6483,#6484,#6485,#6486,#6487,#6488,#6489,
#6490,#6491,#6492,#6493,#6494,#6495,#6496,#6497,#6498,#6499,#6500,#6501,
#6502,#6503));
#6551=CLOSED_SHELL('',(#6504,#6505,#6506,#6507,#6508,#6509,#6510,#6511,
#6512,#6513,#6514,#6515,#6516,#6517,#6518,#6519,#6520,#6521,#6522,#6523,
#6524,#6525,#6526,#6527,#6528,#6529,#6530,#6531,#6532,#6533,#6534,#6535,
#6536,#6537,#6538,#6539));
#6552=CLOSED_SHELL('',(#6540,#6541,#6542,#6543));
#6553=DERIVED_UNIT_ELEMENT(#6571,1.);
#6554=DERIVED_UNIT_ELEMENT(#18582,-3.);
#6555=DERIVED_UNIT_ELEMENT(#6571,1.);
#6556=DERIVED_UNIT_ELEMENT(#18582,-3.);
#6557=DERIVED_UNIT_ELEMENT(#6571,1.);
#6558=DERIVED_UNIT_ELEMENT(#18582,-3.);
#6559=DERIVED_UNIT_ELEMENT(#6571,1.);
#6560=DERIVED_UNIT_ELEMENT(#18582,-3.);
#6561=DERIVED_UNIT_ELEMENT(#6571,1.);
#6562=DERIVED_UNIT_ELEMENT(#18582,-3.);
#6563=DERIVED_UNIT_ELEMENT(#6571,1.);
#6564=DERIVED_UNIT_ELEMENT(#18582,-3.);
#6565=DERIVED_UNIT_ELEMENT(#6571,1.);
#6566=DERIVED_UNIT_ELEMENT(#18582,-3.);
#6567=DERIVED_UNIT_ELEMENT(#6571,1.);
#6568=DERIVED_UNIT_ELEMENT(#18582,-3.);
#6569=DERIVED_UNIT_ELEMENT(#6571,1.);
#6570=DERIVED_UNIT_ELEMENT(#18582,-3.);
#6571=(
MASS_UNIT()
NAMED_UNIT(*)
SI_UNIT(.KILO.,.GRAM.)
);
#6572=DERIVED_UNIT((#6553,#6554));
#6573=DERIVED_UNIT((#6555,#6556));
#6574=DERIVED_UNIT((#6557,#6558));
#6575=DERIVED_UNIT((#6559,#6560));
#6576=DERIVED_UNIT((#6561,#6562));
#6577=DERIVED_UNIT((#6563,#6564));
#6578=DERIVED_UNIT((#6565,#6566));
#6579=DERIVED_UNIT((#6567,#6568));
#6580=DERIVED_UNIT((#6569,#6570));
#6581=MEASURE_REPRESENTATION_ITEM('density measure',
POSITIVE_RATIO_MEASURE(7850.),#6572);
#6582=MEASURE_REPRESENTATION_ITEM('density measure',
POSITIVE_RATIO_MEASURE(7850.),#6573);
#6583=MEASURE_REPRESENTATION_ITEM('density measure',
POSITIVE_RATIO_MEASURE(7850.),#6574);
#6584=MEASURE_REPRESENTATION_ITEM('density measure',
POSITIVE_RATIO_MEASURE(7850.),#6575);
#6585=MEASURE_REPRESENTATION_ITEM('density measure',
POSITIVE_RATIO_MEASURE(7850.),#6576);
#6586=MEASURE_REPRESENTATION_ITEM('density measure',
POSITIVE_RATIO_MEASURE(7850.),#6577);
#6587=MEASURE_REPRESENTATION_ITEM('density measure',
POSITIVE_RATIO_MEASURE(7850.),#6578);
#6588=MEASURE_REPRESENTATION_ITEM('density measure',
POSITIVE_RATIO_MEASURE(7850.),#6579);
#6589=MEASURE_REPRESENTATION_ITEM('density measure',
POSITIVE_RATIO_MEASURE(7850.),#6580);
#6590=PROPERTY_DEFINITION_REPRESENTATION(#6635,#6608);
#6591=PROPERTY_DEFINITION_REPRESENTATION(#6636,#6609);
#6592=PROPERTY_DEFINITION_REPRESENTATION(#6637,#6610);
#6593=PROPERTY_DEFINITION_REPRESENTATION(#6638,#6611);
#6594=PROPERTY_DEFINITION_REPRESENTATION(#6639,#6612);
#6595=PROPERTY_DEFINITION_REPRESENTATION(#6640,#6613);
#6596=PROPERTY_DEFINITION_REPRESENTATION(#6641,#6614);
#6597=PROPERTY_DEFINITION_REPRESENTATION(#6642,#6615);
#6598=PROPERTY_DEFINITION_REPRESENTATION(#6643,#6616);
#6599=PROPERTY_DEFINITION_REPRESENTATION(#6644,#6617);
#6600=PROPERTY_DEFINITION_REPRESENTATION(#6645,#6618);
#6601=PROPERTY_DEFINITION_REPRESENTATION(#6646,#6619);
#6602=PROPERTY_DEFINITION_REPRESENTATION(#6647,#6620);
#6603=PROPERTY_DEFINITION_REPRESENTATION(#6648,#6621);
#6604=PROPERTY_DEFINITION_REPRESENTATION(#6649,#6622);
#6605=PROPERTY_DEFINITION_REPRESENTATION(#6650,#6623);
#6606=PROPERTY_DEFINITION_REPRESENTATION(#6651,#6624);
#6607=PROPERTY_DEFINITION_REPRESENTATION(#6652,#6625);
#6608=REPRESENTATION('material name',(#6626),#18570);
#6609=REPRESENTATION('density',(#6581),#18570);
#6610=REPRESENTATION('material name',(#6627),#18571);
#6611=REPRESENTATION('density',(#6582),#18571);
#6612=REPRESENTATION('material name',(#6628),#18572);
#6613=REPRESENTATION('density',(#6583),#18572);
#6614=REPRESENTATION('material name',(#6629),#18574);
#6615=REPRESENTATION('density',(#6584),#18574);
#6616=REPRESENTATION('material name',(#6630),#18575);
#6617=REPRESENTATION('density',(#6585),#18575);
#6618=REPRESENTATION('material name',(#6631),#18576);
#6619=REPRESENTATION('density',(#6586),#18576);
#6620=REPRESENTATION('material name',(#6632),#18577);
#6621=REPRESENTATION('density',(#6587),#18577);
#6622=REPRESENTATION('material name',(#6633),#18578);
#6623=REPRESENTATION('density',(#6588),#18578);
#6624=REPRESENTATION('material name',(#6634),#18579);
#6625=REPRESENTATION('density',(#6589),#18579);
#6626=DESCRIPTIVE_REPRESENTATION_ITEM('Steel','Steel');
#6627=DESCRIPTIVE_REPRESENTATION_ITEM('Steel','Steel');
#6628=DESCRIPTIVE_REPRESENTATION_ITEM('Steel','Steel');
#6629=DESCRIPTIVE_REPRESENTATION_ITEM('Steel','Steel');
#6630=DESCRIPTIVE_REPRESENTATION_ITEM('Steel','Steel');
#6631=DESCRIPTIVE_REPRESENTATION_ITEM('Steel','Steel');
#6632=DESCRIPTIVE_REPRESENTATION_ITEM('Steel','Steel');
#6633=DESCRIPTIVE_REPRESENTATION_ITEM('Steel','Steel');
#6634=DESCRIPTIVE_REPRESENTATION_ITEM('Steel','Steel');
#6635=PROPERTY_DEFINITION('material property','material name',#18636);
#6636=PROPERTY_DEFINITION('material property','density of part',#18636);
#6637=PROPERTY_DEFINITION('material property','material name',#18637);
#6638=PROPERTY_DEFINITION('material property','density of part',#18637);
#6639=PROPERTY_DEFINITION('material property','material name',#18638);
#6640=PROPERTY_DEFINITION('material property','density of part',#18638);
#6641=PROPERTY_DEFINITION('material property','material name',#18640);
#6642=PROPERTY_DEFINITION('material property','density of part',#18640);
#6643=PROPERTY_DEFINITION('material property','material name',#18641);
#6644=PROPERTY_DEFINITION('material property','density of part',#18641);
#6645=PROPERTY_DEFINITION('material property','material name',#18642);
#6646=PROPERTY_DEFINITION('material property','density of part',#18642);
#6647=PROPERTY_DEFINITION('material property','material name',#18643);
#6648=PROPERTY_DEFINITION('material property','density of part',#18643);
#6649=PROPERTY_DEFINITION('material property','material name',#18644);
#6650=PROPERTY_DEFINITION('material property','density of part',#18644);
#6651=PROPERTY_DEFINITION('material property','material name',#18645);
#6652=PROPERTY_DEFINITION('material property','density of part',#18645);
#6653=AXIS2_PLACEMENT_3D('',#8503,#7134,#7135);
#6654=AXIS2_PLACEMENT_3D('',#8504,#7136,#7137);
#6655=AXIS2_PLACEMENT_3D('',#8505,#7138,#7139);
#6656=AXIS2_PLACEMENT_3D('',#8507,#7140,#7141);
#6657=AXIS2_PLACEMENT_3D('',#8510,#7143,#7144);
#6658=AXIS2_PLACEMENT_3D('',#8511,#7145,#7146);
#6659=AXIS2_PLACEMENT_3D('',#8513,#7147,#7148);
#6660=AXIS2_PLACEMENT_3D('',#8516,#7150,#7151);
#6661=AXIS2_PLACEMENT_3D('',#8517,#7152,#7153);
#6662=AXIS2_PLACEMENT_3D('',#8519,#7154,#7155);
#6663=AXIS2_PLACEMENT_3D('',#8522,#7157,#7158);
#6664=AXIS2_PLACEMENT_3D('',#8523,#7159,#7160);
#6665=AXIS2_PLACEMENT_3D('',#8530,#7164,#7165);
#6666=AXIS2_PLACEMENT_3D('',#8538,#7170,#7171);
#6667=AXIS2_PLACEMENT_3D('',#8544,#7175,#7176);
#6668=AXIS2_PLACEMENT_3D('',#8548,#7179,#7180);
#6669=AXIS2_PLACEMENT_3D('',#8558,#7186,#7187);
#6670=AXIS2_PLACEMENT_3D('',#8564,#7191,#7192);
#6671=AXIS2_PLACEMENT_3D('',#8568,#7195,#7196);
#6672=AXIS2_PLACEMENT_3D('',#8572,#7199,#7200);
#6673=AXIS2_PLACEMENT_3D('',#8576,#7203,#7204);
#6674=AXIS2_PLACEMENT_3D('',#8578,#7206,#7207);
#6675=AXIS2_PLACEMENT_3D('',#8586,#7211,#7212);
#6676=AXIS2_PLACEMENT_3D('',#8600,#7219,#7220);
#6677=AXIS2_PLACEMENT_3D('',#8604,#7223,#7224);
#6678=AXIS2_PLACEMENT_3D('',#8610,#7228,#7229);
#6679=AXIS2_PLACEMENT_3D('',#8614,#7232,#7233);
#6680=AXIS2_PLACEMENT_3D('',#8618,#7236,#7237);
#6681=AXIS2_PLACEMENT_3D('',#8622,#7240,#7241);
#6682=AXIS2_PLACEMENT_3D('',#8625,#7243,#7244);
#6683=AXIS2_PLACEMENT_3D('',#8626,#7245,#7246);
#6684=AXIS2_PLACEMENT_3D('',#8628,#7247,#7248);
#6685=AXIS2_PLACEMENT_3D('',#8630,#7250,#7251);
#6686=AXIS2_PLACEMENT_3D('',#8642,#7258,#7259);
#6687=AXIS2_PLACEMENT_3D('',#8644,#7261,#7262);
#6688=AXIS2_PLACEMENT_3D('',#8646,#7264,#7265);
#6689=AXIS2_PLACEMENT_3D('',#8648,#7267,#7268);
#6690=AXIS2_PLACEMENT_3D('',#8650,#7270,#7271);
#6691=AXIS2_PLACEMENT_3D('',#8652,#7273,#7274);
#6692=AXIS2_PLACEMENT_3D('',#8653,#7275,#7276);
#6693=AXIS2_PLACEMENT_3D('',#8654,#7277,#7278);
#6694=AXIS2_PLACEMENT_3D('',#8656,#7279,#7280);
#6695=AXIS2_PLACEMENT_3D('',#8659,#7282,#7283);
#6696=AXIS2_PLACEMENT_3D('',#8660,#7284,#7285);
#6697=AXIS2_PLACEMENT_3D('',#8662,#7286,#7287);
#6698=AXIS2_PLACEMENT_3D('',#8663,#7288,#7289);
#6699=AXIS2_PLACEMENT_3D('',#8665,#7290,#7291);
#6700=AXIS2_PLACEMENT_3D('',#8666,#7292,#7293);
#6701=AXIS2_PLACEMENT_3D('',#8668,#7294,#7295);
#6702=AXIS2_PLACEMENT_3D('',#8670,#7297,#7298);
#6703=AXIS2_PLACEMENT_3D('',#8672,#7299,#7300);
#6704=AXIS2_PLACEMENT_3D('',#8674,#7301,#7302);
#6705=AXIS2_PLACEMENT_3D('',#8675,#7303,#7304);
#6706=AXIS2_PLACEMENT_3D('',#8678,#7306,#7307);
#6707=AXIS2_PLACEMENT_3D('',#8679,#7308,#7309);
#6708=AXIS2_PLACEMENT_3D('',#8680,#7310,#7311);
#6709=AXIS2_PLACEMENT_3D('',#8682,#7313,#7314);
#6710=AXIS2_PLACEMENT_3D('',#8683,#7315,#7316);
#6711=AXIS2_PLACEMENT_3D('',#8684,#7317,#7318);
#6712=AXIS2_PLACEMENT_3D('',#8693,#7323,#7324);
#6713=AXIS2_PLACEMENT_3D('',#8702,#7329,#7330);
#6714=AXIS2_PLACEMENT_3D('',#8703,#7331,#7332);
#6715=AXIS2_PLACEMENT_3D('',#8704,#7333,#7334);
#6716=AXIS2_PLACEMENT_3D('',#8705,#7335,#7336);
#6717=AXIS2_PLACEMENT_3D('',#8706,#7337,#7338);
#6718=AXIS2_PLACEMENT_3D('',#8707,#7339,#7340);
#6719=AXIS2_PLACEMENT_3D('',#8708,#7341,#7342);
#6720=AXIS2_PLACEMENT_3D('',#8709,#7343,#7344);
#6721=AXIS2_PLACEMENT_3D('',#8710,#7345,#7346);
#6722=AXIS2_PLACEMENT_3D('',#8711,#7347,#7348);
#6723=AXIS2_PLACEMENT_3D('',#8712,#7349,#7350);
#6724=AXIS2_PLACEMENT_3D('',#8739,#7351,#7352);
#6725=AXIS2_PLACEMENT_3D('',#8740,#7353,#7354);
#6726=AXIS2_PLACEMENT_3D('',#8763,#7355,#7356);
#6727=AXIS2_PLACEMENT_3D('',#8764,#7357,#7358);
#6728=AXIS2_PLACEMENT_3D('',#8787,#7359,#7360);
#6729=AXIS2_PLACEMENT_3D('',#8788,#7361,#7362);
#6730=AXIS2_PLACEMENT_3D('',#8815,#7363,#7364);
#6731=AXIS2_PLACEMENT_3D('',#9000,#7365,#7366);
#6732=AXIS2_PLACEMENT_3D('',#9014,#7369,#7370);
#6733=AXIS2_PLACEMENT_3D('',#9016,#7371,#7372);
#6734=AXIS2_PLACEMENT_3D('',#9018,#7373,#7374);
#6735=AXIS2_PLACEMENT_3D('',#9019,#7375,#7376);
#6736=AXIS2_PLACEMENT_3D('',#9021,#7377,#7378);
#6737=AXIS2_PLACEMENT_3D('',#9023,#7380,#7381);
#6738=AXIS2_PLACEMENT_3D('',#9025,#7382,#7383);
#6739=AXIS2_PLACEMENT_3D('',#9028,#7385,#7386);
#6740=AXIS2_PLACEMENT_3D('',#9029,#7387,#7388);
#6741=AXIS2_PLACEMENT_3D('',#9031,#7389,#7390);
#6742=AXIS2_PLACEMENT_3D('',#9034,#7392,#7393);
#6743=AXIS2_PLACEMENT_3D('',#9035,#7394,#7395);
#6744=AXIS2_PLACEMENT_3D('',#9037,#7396,#7397);
#6745=AXIS2_PLACEMENT_3D('',#9039,#7399,#7400);
#6746=AXIS2_PLACEMENT_3D('',#9041,#7401,#7402);
#6747=AXIS2_PLACEMENT_3D('',#9044,#7404,#7405);
#6748=AXIS2_PLACEMENT_3D('',#9045,#7406,#7407);
#6749=AXIS2_PLACEMENT_3D('',#9047,#7408,#7409);
#6750=AXIS2_PLACEMENT_3D('',#9048,#7410,#7411);
#6751=AXIS2_PLACEMENT_3D('',#9050,#7412,#7413);
#6752=AXIS2_PLACEMENT_3D('',#9053,#7415,#7416);
#6753=AXIS2_PLACEMENT_3D('',#9054,#7417,#7418);
#6754=AXIS2_PLACEMENT_3D('',#9056,#7419,#7420);
#6755=AXIS2_PLACEMENT_3D('',#9057,#7421,#7422);
#6756=AXIS2_PLACEMENT_3D('',#9060,#7424,#7425);
#6757=AXIS2_PLACEMENT_3D('',#9061,#7426,#7427);
#6758=AXIS2_PLACEMENT_3D('',#9064,#7429,#7430);
#6759=AXIS2_PLACEMENT_3D('',#9065,#7431,#7432);
#6760=AXIS2_PLACEMENT_3D('',#9074,#7437,#7438);
#6761=AXIS2_PLACEMENT_3D('',#9083,#7443,#7444);
#6762=AXIS2_PLACEMENT_3D('',#9092,#7449,#7450);
#6763=AXIS2_PLACEMENT_3D('',#9101,#7455,#7456);
#6764=AXIS2_PLACEMENT_3D('',#9110,#7461,#7462);
#6765=AXIS2_PLACEMENT_3D('',#9119,#7467,#7468);
#6766=AXIS2_PLACEMENT_3D('',#9128,#7473,#7474);
#6767=AXIS2_PLACEMENT_3D('',#9130,#7475,#7476);
#6768=AXIS2_PLACEMENT_3D('',#9131,#7477,#7478);
#6769=AXIS2_PLACEMENT_3D('',#9133,#7479,#7480);
#6770=AXIS2_PLACEMENT_3D('',#9134,#7481,#7482);
#6771=AXIS2_PLACEMENT_3D('',#9137,#7485,#7486);
#6772=AXIS2_PLACEMENT_3D('',#9140,#7489,#7490);
#6773=AXIS2_PLACEMENT_3D('',#9143,#7493,#7494);
#6774=AXIS2_PLACEMENT_3D('',#9149,#7498,#7499);
#6775=AXIS2_PLACEMENT_3D('',#9155,#7503,#7504);
#6776=AXIS2_PLACEMENT_3D('',#9200,#7506,#7507);
#6777=AXIS2_PLACEMENT_3D('',#9246,#7510,#7511);
#6778=AXIS2_PLACEMENT_3D('',#9324,#7515,#7516);
#6779=AXIS2_PLACEMENT_3D('',#9372,#7520,#7521);
#6780=AXIS2_PLACEMENT_3D('',#9388,#7525,#7526);
#6781=AXIS2_PLACEMENT_3D('',#9709,#7538,#7539);
#6782=AXIS2_PLACEMENT_3D('',#9711,#7541,#7542);
#6783=AXIS2_PLACEMENT_3D('',#9713,#7543,#7544);
#6784=AXIS2_PLACEMENT_3D('',#9715,#7546,#7547);
#6785=AXIS2_PLACEMENT_3D('',#9879,#7549,#7550);
#6786=AXIS2_PLACEMENT_3D('',#9880,#7551,#7552);
#6787=AXIS2_PLACEMENT_3D('',#9928,#7554,#7555);
#6788=AXIS2_PLACEMENT_3D('',#10046,#7557,#7558);
#6789=AXIS2_PLACEMENT_3D('',#10091,#7559,#7560);
#6790=AXIS2_PLACEMENT_3D('',#10183,#7562,#7563);
#6791=AXIS2_PLACEMENT_3D('',#10200,#7564,#7565);
#6792=AXIS2_PLACEMENT_3D('',#10320,#7567,#7568);
#6793=AXIS2_PLACEMENT_3D('',#10325,#7569,#7570);
#6794=AXIS2_PLACEMENT_3D('',#10377,#7572,#7573);
#6795=AXIS2_PLACEMENT_3D('',#10378,#7574,#7575);
#6796=AXIS2_PLACEMENT_3D('',#10379,#7576,#7577);
#6797=AXIS2_PLACEMENT_3D('',#10380,#7578,#7579);
#6798=AXIS2_PLACEMENT_3D('',#10381,#7580,#7581);
#6799=AXIS2_PLACEMENT_3D('',#10382,#7582,#7583);
#6800=AXIS2_PLACEMENT_3D('',#10384,#7584,#7585);
#6801=AXIS2_PLACEMENT_3D('',#10385,#7586,#7587);
#6802=AXIS2_PLACEMENT_3D('',#10386,#7588,#7589);
#6803=AXIS2_PLACEMENT_3D('',#10387,#7590,#7591);
#6804=AXIS2_PLACEMENT_3D('',#10388,#7592,#7593);
#6805=AXIS2_PLACEMENT_3D('',#10389,#7594,#7595);
#6806=AXIS2_PLACEMENT_3D('',#10410,#7596,#7597);
#6807=AXIS2_PLACEMENT_3D('',#10412,#7598,#7599);
#6808=AXIS2_PLACEMENT_3D('',#10413,#7600,#7601);
#6809=AXIS2_PLACEMENT_3D('',#10414,#7602,#7603);
#6810=AXIS2_PLACEMENT_3D('',#10504,#7605,#7606);
#6811=AXIS2_PLACEMENT_3D('',#10505,#7607,#7608);
#6812=AXIS2_PLACEMENT_3D('',#10508,#7609,#7610);
#6813=AXIS2_PLACEMENT_3D('',#10510,#7611,#7612);
#6814=AXIS2_PLACEMENT_3D('',#10511,#7613,#7614);
#6815=AXIS2_PLACEMENT_3D('',#10512,#7615,#7616);
#6816=AXIS2_PLACEMENT_3D('',#10515,#7617,#7618);
#6817=AXIS2_PLACEMENT_3D('',#10517,#7619,#7620);
#6818=AXIS2_PLACEMENT_3D('',#10518,#7621,#7622);
#6819=AXIS2_PLACEMENT_3D('',#10519,#7623,#7624);
#6820=AXIS2_PLACEMENT_3D('',#10522,#7625,#7626);
#6821=AXIS2_PLACEMENT_3D('',#10524,#7627,#7628);
#6822=AXIS2_PLACEMENT_3D('',#10525,#7629,#7630);
#6823=AXIS2_PLACEMENT_3D('',#10526,#7631,#7632);
#6824=AXIS2_PLACEMENT_3D('',#10557,#7635,#7636);
#6825=AXIS2_PLACEMENT_3D('',#10560,#7637,#7638);
#6826=AXIS2_PLACEMENT_3D('',#10562,#7639,#7640);
#6827=AXIS2_PLACEMENT_3D('',#10563,#7641,#7642);
#6828=AXIS2_PLACEMENT_3D('',#10564,#7643,#7644);
#6829=AXIS2_PLACEMENT_3D('',#10737,#7647,#7648);
#6830=AXIS2_PLACEMENT_3D('',#10738,#7649,#7650);
#6831=AXIS2_PLACEMENT_3D('',#10755,#7651,#7652);
#6832=AXIS2_PLACEMENT_3D('',#10756,#7653,#7654);
#6833=AXIS2_PLACEMENT_3D('',#10757,#7655,#7656);
#6834=AXIS2_PLACEMENT_3D('',#10784,#7657,#7658);
#6835=AXIS2_PLACEMENT_3D('',#10785,#7659,#7660);
#6836=AXIS2_PLACEMENT_3D('',#10808,#7661,#7662);
#6837=AXIS2_PLACEMENT_3D('',#10809,#7663,#7664);
#6838=AXIS2_PLACEMENT_3D('',#10832,#7665,#7666);
#6839=AXIS2_PLACEMENT_3D('',#10833,#7667,#7668);
#6840=AXIS2_PLACEMENT_3D('',#10860,#7669,#7670);
#6841=AXIS2_PLACEMENT_3D('',#11045,#7671,#7672);
#6842=AXIS2_PLACEMENT_3D('',#11059,#7675,#7676);
#6843=AXIS2_PLACEMENT_3D('',#11061,#7677,#7678);
#6844=AXIS2_PLACEMENT_3D('',#11063,#7679,#7680);
#6845=AXIS2_PLACEMENT_3D('',#11064,#7681,#7682);
#6846=AXIS2_PLACEMENT_3D('',#11073,#7687,#7688);
#6847=AXIS2_PLACEMENT_3D('',#11079,#7692,#7693);
#6848=AXIS2_PLACEMENT_3D('',#11085,#7697,#7698);
#6849=AXIS2_PLACEMENT_3D('',#11091,#7702,#7703);
#6850=AXIS2_PLACEMENT_3D('',#11097,#7707,#7708);
#6851=AXIS2_PLACEMENT_3D('',#11100,#7711,#7712);
#6852=AXIS2_PLACEMENT_3D('',#11102,#7713,#7714);
#6853=AXIS2_PLACEMENT_3D('',#11103,#7715,#7716);
#6854=AXIS2_PLACEMENT_3D('',#11112,#7721,#7722);
#6855=AXIS2_PLACEMENT_3D('',#11118,#7726,#7727);
#6856=AXIS2_PLACEMENT_3D('',#11124,#7731,#7732);
#6857=AXIS2_PLACEMENT_3D('',#11130,#7736,#7737);
#6858=AXIS2_PLACEMENT_3D('',#11136,#7741,#7742);
#6859=AXIS2_PLACEMENT_3D('',#11139,#7745,#7746);
#6860=AXIS2_PLACEMENT_3D('',#11141,#7747,#7748);
#6861=AXIS2_PLACEMENT_3D('',#11142,#7749,#7750);
#6862=AXIS2_PLACEMENT_3D('',#11144,#7751,#7752);
#6863=AXIS2_PLACEMENT_3D('',#11146,#7754,#7755);
#6864=AXIS2_PLACEMENT_3D('',#11148,#7756,#7757);
#6865=AXIS2_PLACEMENT_3D('',#11151,#7759,#7760);
#6866=AXIS2_PLACEMENT_3D('',#11152,#7761,#7762);
#6867=AXIS2_PLACEMENT_3D('',#11154,#7763,#7764);
#6868=AXIS2_PLACEMENT_3D('',#11157,#7766,#7767);
#6869=AXIS2_PLACEMENT_3D('',#11158,#7768,#7769);
#6870=AXIS2_PLACEMENT_3D('',#11160,#7770,#7771);
#6871=AXIS2_PLACEMENT_3D('',#11162,#7773,#7774);
#6872=AXIS2_PLACEMENT_3D('',#11165,#7776,#7777);
#6873=AXIS2_PLACEMENT_3D('',#11166,#7778,#7779);
#6874=AXIS2_PLACEMENT_3D('',#11169,#7781,#7782);
#6875=AXIS2_PLACEMENT_3D('',#11170,#7783,#7784);
#6876=AXIS2_PLACEMENT_3D('',#11179,#7789,#7790);
#6877=AXIS2_PLACEMENT_3D('',#11188,#7795,#7796);
#6878=AXIS2_PLACEMENT_3D('',#11197,#7801,#7802);
#6879=AXIS2_PLACEMENT_3D('',#11206,#7807,#7808);
#6880=AXIS2_PLACEMENT_3D('',#11215,#7813,#7814);
#6881=AXIS2_PLACEMENT_3D('',#11224,#7819,#7820);
#6882=AXIS2_PLACEMENT_3D('',#11233,#7825,#7826);
#6883=AXIS2_PLACEMENT_3D('',#11235,#7827,#7828);
#6884=AXIS2_PLACEMENT_3D('',#11236,#7829,#7830);
#6885=AXIS2_PLACEMENT_3D('',#11238,#7831,#7832);
#6886=AXIS2_PLACEMENT_3D('',#11239,#7833,#7834);
#6887=AXIS2_PLACEMENT_3D('',#11242,#7837,#7838);
#6888=AXIS2_PLACEMENT_3D('',#11245,#7841,#7842);
#6889=AXIS2_PLACEMENT_3D('',#11248,#7845,#7846);
#6890=AXIS2_PLACEMENT_3D('',#11254,#7850,#7851);
#6891=AXIS2_PLACEMENT_3D('',#11260,#7855,#7856);
#6892=AXIS2_PLACEMENT_3D('',#11305,#7858,#7859);
#6893=AXIS2_PLACEMENT_3D('',#11351,#7862,#7863);
#6894=AXIS2_PLACEMENT_3D('',#11429,#7867,#7868);
#6895=AXIS2_PLACEMENT_3D('',#11477,#7872,#7873);
#6896=AXIS2_PLACEMENT_3D('',#11493,#7877,#7878);
#6897=AXIS2_PLACEMENT_3D('',#11814,#7890,#7891);
#6898=AXIS2_PLACEMENT_3D('',#11816,#7893,#7894);
#6899=AXIS2_PLACEMENT_3D('',#11818,#7895,#7896);
#6900=AXIS2_PLACEMENT_3D('',#11820,#7898,#7899);
#6901=AXIS2_PLACEMENT_3D('',#11984,#7901,#7902);
#6902=AXIS2_PLACEMENT_3D('',#11985,#7903,#7904);
#6903=AXIS2_PLACEMENT_3D('',#12033,#7906,#7907);
#6904=AXIS2_PLACEMENT_3D('',#12151,#7909,#7910);
#6905=AXIS2_PLACEMENT_3D('',#12196,#7911,#7912);
#6906=AXIS2_PLACEMENT_3D('',#12288,#7914,#7915);
#6907=AXIS2_PLACEMENT_3D('',#12305,#7916,#7917);
#6908=AXIS2_PLACEMENT_3D('',#12425,#7919,#7920);
#6909=AXIS2_PLACEMENT_3D('',#12430,#7921,#7922);
#6910=AXIS2_PLACEMENT_3D('',#12482,#7924,#7925);
#6911=AXIS2_PLACEMENT_3D('',#12483,#7926,#7927);
#6912=AXIS2_PLACEMENT_3D('',#12484,#7928,#7929);
#6913=AXIS2_PLACEMENT_3D('',#12485,#7930,#7931);
#6914=AXIS2_PLACEMENT_3D('',#12486,#7932,#7933);
#6915=AXIS2_PLACEMENT_3D('',#12487,#7934,#7935);
#6916=AXIS2_PLACEMENT_3D('',#12489,#7936,#7937);
#6917=AXIS2_PLACEMENT_3D('',#12490,#7938,#7939);
#6918=AXIS2_PLACEMENT_3D('',#12491,#7940,#7941);
#6919=AXIS2_PLACEMENT_3D('',#12492,#7942,#7943);
#6920=AXIS2_PLACEMENT_3D('',#12493,#7944,#7945);
#6921=AXIS2_PLACEMENT_3D('',#12494,#7946,#7947);
#6922=AXIS2_PLACEMENT_3D('',#12515,#7948,#7949);
#6923=AXIS2_PLACEMENT_3D('',#12517,#7950,#7951);
#6924=AXIS2_PLACEMENT_3D('',#12518,#7952,#7953);
#6925=AXIS2_PLACEMENT_3D('',#12519,#7954,#7955);
#6926=AXIS2_PLACEMENT_3D('',#12609,#7957,#7958);
#6927=AXIS2_PLACEMENT_3D('',#12610,#7959,#7960);
#6928=AXIS2_PLACEMENT_3D('',#12613,#7961,#7962);
#6929=AXIS2_PLACEMENT_3D('',#12615,#7963,#7964);
#6930=AXIS2_PLACEMENT_3D('',#12616,#7965,#7966);
#6931=AXIS2_PLACEMENT_3D('',#12617,#7967,#7968);
#6932=AXIS2_PLACEMENT_3D('',#12620,#7969,#7970);
#6933=AXIS2_PLACEMENT_3D('',#12622,#7971,#7972);
#6934=AXIS2_PLACEMENT_3D('',#12623,#7973,#7974);
#6935=AXIS2_PLACEMENT_3D('',#12624,#7975,#7976);
#6936=AXIS2_PLACEMENT_3D('',#12627,#7977,#7978);
#6937=AXIS2_PLACEMENT_3D('',#12629,#7979,#7980);
#6938=AXIS2_PLACEMENT_3D('',#12630,#7981,#7982);
#6939=AXIS2_PLACEMENT_3D('',#12631,#7983,#7984);
#6940=AXIS2_PLACEMENT_3D('',#12662,#7987,#7988);
#6941=AXIS2_PLACEMENT_3D('',#12665,#7989,#7990);
#6942=AXIS2_PLACEMENT_3D('',#12667,#7991,#7992);
#6943=AXIS2_PLACEMENT_3D('',#12668,#7993,#7994);
#6944=AXIS2_PLACEMENT_3D('',#12669,#7995,#7996);
#6945=AXIS2_PLACEMENT_3D('',#12842,#7999,#8000);
#6946=AXIS2_PLACEMENT_3D('',#12843,#8001,#8002);
#6947=AXIS2_PLACEMENT_3D('',#12860,#8003,#8004);
#6948=AXIS2_PLACEMENT_3D('',#12861,#8005,#8006);
#6949=AXIS2_PLACEMENT_3D('',#12862,#8007,#8008);
#6950=AXIS2_PLACEMENT_3D('',#12878,#8010,#8011);
#6951=AXIS2_PLACEMENT_3D('',#12886,#8012,#8013);
#6952=AXIS2_PLACEMENT_3D('',#12934,#8015,#8016);
#6953=AXIS2_PLACEMENT_3D('',#12982,#8018,#8019);
#6954=AXIS2_PLACEMENT_3D('',#13033,#8021,#8022);
#6955=AXIS2_PLACEMENT_3D('',#13081,#8024,#8025);
#6956=AXIS2_PLACEMENT_3D('',#13129,#8027,#8028);
#6957=AXIS2_PLACEMENT_3D('',#13177,#8030,#8031);
#6958=AXIS2_PLACEMENT_3D('',#13231,#8033,#8034);
#6959=AXIS2_PLACEMENT_3D('',#13279,#8036,#8037);
#6960=AXIS2_PLACEMENT_3D('',#13327,#8039,#8040);
#6961=AXIS2_PLACEMENT_3D('',#13381,#8042,#8043);
#6962=AXIS2_PLACEMENT_3D('',#13429,#8045,#8046);
#6963=AXIS2_PLACEMENT_3D('',#13477,#8048,#8049);
#6964=AXIS2_PLACEMENT_3D('',#13525,#8051,#8052);
#6965=AXIS2_PLACEMENT_3D('',#13579,#8054,#8055);
#6966=AXIS2_PLACEMENT_3D('',#13627,#8057,#8058);
#6967=AXIS2_PLACEMENT_3D('',#13675,#8060,#8061);
#6968=AXIS2_PLACEMENT_3D('',#13729,#8063,#8064);
#6969=AXIS2_PLACEMENT_3D('',#13777,#8066,#8067);
#6970=AXIS2_PLACEMENT_3D('',#13825,#8069,#8070);
#6971=AXIS2_PLACEMENT_3D('',#13879,#8072,#8073);
#6972=AXIS2_PLACEMENT_3D('',#13927,#8075,#8076);
#6973=AXIS2_PLACEMENT_3D('',#13975,#8078,#8079);
#6974=AXIS2_PLACEMENT_3D('',#14023,#8081,#8082);
#6975=AXIS2_PLACEMENT_3D('',#14077,#8084,#8085);
#6976=AXIS2_PLACEMENT_3D('',#14125,#8087,#8088);
#6977=AXIS2_PLACEMENT_3D('',#14173,#8090,#8091);
#6978=AXIS2_PLACEMENT_3D('',#14227,#8093,#8094);
#6979=AXIS2_PLACEMENT_3D('',#14275,#8096,#8097);
#6980=AXIS2_PLACEMENT_3D('',#14323,#8099,#8100);
#6981=AXIS2_PLACEMENT_3D('',#14339,#8102,#8103);
#6982=AXIS2_PLACEMENT_3D('',#14349,#8104,#8105);
#6983=AXIS2_PLACEMENT_3D('',#14373,#8107,#8108);
#6984=AXIS2_PLACEMENT_3D('',#14397,#8110,#8111);
#6985=AXIS2_PLACEMENT_3D('',#14422,#8113,#8114);
#6986=AXIS2_PLACEMENT_3D('',#14447,#8116,#8117);
#6987=AXIS2_PLACEMENT_3D('',#14471,#8119,#8120);
#6988=AXIS2_PLACEMENT_3D('',#14496,#8122,#8123);
#6989=AXIS2_PLACEMENT_3D('',#14521,#8125,#8126);
#6990=AXIS2_PLACEMENT_3D('',#14545,#8128,#8129);
#6991=AXIS2_PLACEMENT_3D('',#14569,#8131,#8132);
#6992=AXIS2_PLACEMENT_3D('',#14594,#8134,#8135);
#6993=AXIS2_PLACEMENT_3D('',#14619,#8137,#8138);
#6994=AXIS2_PLACEMENT_3D('',#14643,#8140,#8141);
#6995=AXIS2_PLACEMENT_3D('',#14668,#8143,#8144);
#6996=AXIS2_PLACEMENT_3D('',#14693,#8146,#8147);
#6997=AXIS2_PLACEMENT_3D('',#14717,#8149,#8150);
#6998=AXIS2_PLACEMENT_3D('',#14742,#8152,#8153);
#6999=AXIS2_PLACEMENT_3D('',#14767,#8155,#8156);
#7000=AXIS2_PLACEMENT_3D('',#14791,#8158,#8159);
#7001=AXIS2_PLACEMENT_3D('',#14815,#8161,#8162);
#7002=AXIS2_PLACEMENT_3D('',#14840,#8164,#8165);
#7003=AXIS2_PLACEMENT_3D('',#14865,#8167,#8168);
#7004=AXIS2_PLACEMENT_3D('',#14889,#8170,#8171);
#7005=AXIS2_PLACEMENT_3D('',#14914,#8173,#8174);
#7006=AXIS2_PLACEMENT_3D('',#14939,#8176,#8177);
#7007=AXIS2_PLACEMENT_3D('',#14963,#8179,#8180);
#7008=AXIS2_PLACEMENT_3D('',#14988,#8182,#8183);
#7009=AXIS2_PLACEMENT_3D('',#15012,#8185,#8186);
#7010=AXIS2_PLACEMENT_3D('',#15037,#8188,#8189);
#7011=AXIS2_PLACEMENT_3D('',#15061,#8191,#8192);
#7012=AXIS2_PLACEMENT_3D('',#15223,#8193,#8194);
#7013=AXIS2_PLACEMENT_3D('',#15242,#8196,#8197);
#7014=AXIS2_PLACEMENT_3D('',#16104,#8198,#8199);
#7015=AXIS2_PLACEMENT_3D('',#16115,#8200,#8201);
#7016=AXIS2_PLACEMENT_3D('',#16982,#8202,#8203);
#7017=AXIS2_PLACEMENT_3D('',#16983,#8204,#8205);
#7018=AXIS2_PLACEMENT_3D('',#16992,#8210,#8211);
#7019=AXIS2_PLACEMENT_3D('',#16998,#8215,#8216);
#7020=AXIS2_PLACEMENT_3D('',#17004,#8220,#8221);
#7021=AXIS2_PLACEMENT_3D('',#17010,#8225,#8226);
#7022=AXIS2_PLACEMENT_3D('',#17016,#8230,#8231);
#7023=AXIS2_PLACEMENT_3D('',#17019,#8234,#8235);
#7024=AXIS2_PLACEMENT_3D('',#17020,#8236,#8237);
#7025=AXIS2_PLACEMENT_3D('',#17022,#8238,#8239);
#7026=AXIS2_PLACEMENT_3D('',#17023,#8240,#8241);
#7027=AXIS2_PLACEMENT_3D('',#17026,#8243,#8244);
#7028=AXIS2_PLACEMENT_3D('',#17027,#8245,#8246);
#7029=AXIS2_PLACEMENT_3D('',#17028,#8247,#8248);
#7030=AXIS2_PLACEMENT_3D('',#17029,#8249,#8250);
#7031=AXIS2_PLACEMENT_3D('',#17030,#8251,#8252);
#7032=AXIS2_PLACEMENT_3D('',#17035,#8254,#8255);
#7033=AXIS2_PLACEMENT_3D('',#17043,#8256,#8257);
#7034=AXIS2_PLACEMENT_3D('',#17067,#8259,#8260);
#7035=AXIS2_PLACEMENT_3D('',#17090,#8261,#8262);
#7036=AXIS2_PLACEMENT_3D('',#17144,#8264,#8265);
#7037=AXIS2_PLACEMENT_3D('',#17192,#8267,#8268);
#7038=AXIS2_PLACEMENT_3D('',#17211,#8270,#8271);
#7039=AXIS2_PLACEMENT_3D('',#17231,#8272,#8273);
#7040=AXIS2_PLACEMENT_3D('',#17244,#8275,#8276);
#7041=AXIS2_PLACEMENT_3D('',#17252,#8277,#8278);
#7042=AXIS2_PLACEMENT_3D('',#17277,#8280,#8281);
#7043=AXIS2_PLACEMENT_3D('',#17302,#8283,#8284);
#7044=AXIS2_PLACEMENT_3D('',#17327,#8286,#8287);
#7045=AXIS2_PLACEMENT_3D('',#17338,#8289,#8290);
#7046=AXIS2_PLACEMENT_3D('',#17344,#8291,#8292);
#7047=AXIS2_PLACEMENT_3D('',#17900,#8293,#8294);
#7048=AXIS2_PLACEMENT_3D('',#17913,#8301,#8302);
#7049=AXIS2_PLACEMENT_3D('',#17914,#8303,#8304);
#7050=AXIS2_PLACEMENT_3D('',#17920,#8308,#8309);
#7051=AXIS2_PLACEMENT_3D('',#17924,#8312,#8313);
#7052=AXIS2_PLACEMENT_3D('',#17928,#8316,#8317);
#7053=AXIS2_PLACEMENT_3D('',#17932,#8320,#8321);
#7054=AXIS2_PLACEMENT_3D('',#17936,#8324,#8325);
#7055=AXIS2_PLACEMENT_3D('',#17938,#8327,#8328);
#7056=AXIS2_PLACEMENT_3D('',#17939,#8329,#8330);
#7057=AXIS2_PLACEMENT_3D('',#17940,#8331,#8332);
#7058=AXIS2_PLACEMENT_3D('',#17942,#8333,#8334);
#7059=AXIS2_PLACEMENT_3D('',#17945,#8336,#8337);
#7060=AXIS2_PLACEMENT_3D('',#17946,#8338,#8339);
#7061=AXIS2_PLACEMENT_3D('',#17948,#8340,#8341);
#7062=AXIS2_PLACEMENT_3D('',#17951,#8343,#8344);
#7063=AXIS2_PLACEMENT_3D('',#17952,#8345,#8346);
#7064=AXIS2_PLACEMENT_3D('',#17954,#8347,#8348);
#7065=AXIS2_PLACEMENT_3D('',#17956,#8349,#8350);
#7066=AXIS2_PLACEMENT_3D('',#17957,#8351,#8352);
#7067=AXIS2_PLACEMENT_3D('',#17959,#8353,#8354);
#7068=AXIS2_PLACEMENT_3D('',#17961,#8356,#8357);
#7069=AXIS2_PLACEMENT_3D('',#17962,#8358,#8359);
#7070=AXIS2_PLACEMENT_3D('',#17964,#8360,#8361);
#7071=AXIS2_PLACEMENT_3D('',#17966,#8362,#8363);
#7072=AXIS2_PLACEMENT_3D('',#17967,#8364,#8365);
#7073=AXIS2_PLACEMENT_3D('',#17969,#8366,#8367);
#7074=AXIS2_PLACEMENT_3D('',#17971,#8369,#8370);
#7075=AXIS2_PLACEMENT_3D('',#17972,#8371,#8372);
#7076=AXIS2_PLACEMENT_3D('',#17974,#8373,#8374);
#7077=AXIS2_PLACEMENT_3D('',#17976,#8375,#8376);
#7078=AXIS2_PLACEMENT_3D('',#17977,#8377,#8378);
#7079=AXIS2_PLACEMENT_3D('',#17979,#8379,#8380);
#7080=AXIS2_PLACEMENT_3D('',#17981,#8382,#8383);
#7081=AXIS2_PLACEMENT_3D('',#17982,#8384,#8385);
#7082=AXIS2_PLACEMENT_3D('',#17984,#8386,#8387);
#7083=AXIS2_PLACEMENT_3D('',#17986,#8388,#8389);
#7084=AXIS2_PLACEMENT_3D('',#17987,#8390,#8391);
#7085=AXIS2_PLACEMENT_3D('',#17989,#8392,#8393);
#7086=AXIS2_PLACEMENT_3D('',#17991,#8395,#8396);
#7087=AXIS2_PLACEMENT_3D('',#17992,#8397,#8398);
#7088=AXIS2_PLACEMENT_3D('',#17995,#8400,#8401);
#7089=AXIS2_PLACEMENT_3D('',#17996,#8402,#8403);
#7090=AXIS2_PLACEMENT_3D('',#17999,#8405,#8406);
#7091=AXIS2_PLACEMENT_3D('',#18000,#8407,#8408);
#7092=AXIS2_PLACEMENT_3D('',#18003,#8410,#8411);
#7093=AXIS2_PLACEMENT_3D('',#18004,#8412,#8413);
#7094=AXIS2_PLACEMENT_3D('',#18007,#8415,#8416);
#7095=AXIS2_PLACEMENT_3D('',#18035,#8417,#8418);
#7096=AXIS2_PLACEMENT_3D('',#18043,#8419,#8420);
#7097=AXIS2_PLACEMENT_3D('',#18049,#8421,#8422);
#7098=AXIS2_PLACEMENT_3D('',#18052,#8423,#8424);
#7099=AXIS2_PLACEMENT_3D('',#18082,#8427,#8428);
#7100=AXIS2_PLACEMENT_3D('',#18120,#8429,#8430);
#7101=AXIS2_PLACEMENT_3D('',#18158,#8431,#8432);
#7102=AXIS2_PLACEMENT_3D('',#18169,#8433,#8434);
#7103=AXIS2_PLACEMENT_3D('',#18172,#8435,#8436);
#7104=AXIS2_PLACEMENT_3D('',#18202,#8439,#8440);
#7105=AXIS2_PLACEMENT_3D('',#18248,#8441,#8442);
#7106=AXIS2_PLACEMENT_3D('',#18391,#8444,#8445);
#7107=AXIS2_PLACEMENT_3D('',#18392,#8446,#8447);
#7108=AXIS2_PLACEMENT_3D('',#18505,#8449,#8450);
#7109=AXIS2_PLACEMENT_3D('',#18526,#8451,#8452);
#7110=AXIS2_PLACEMENT_3D('',#18527,#8453,#8454);
#7111=AXIS2_PLACEMENT_3D('',#18528,#8455,#8456);
#7112=AXIS2_PLACEMENT_3D('',#18529,#8457,#8458);
#7113=AXIS2_PLACEMENT_3D('',#18530,#8459,#8460);
#7114=AXIS2_PLACEMENT_3D('',#18531,#8461,#8462);
#7115=AXIS2_PLACEMENT_3D('',#18532,#8463,#8464);
#7116=AXIS2_PLACEMENT_3D('',#18533,#8465,#8466);
#7117=AXIS2_PLACEMENT_3D('',#18534,#8467,#8468);
#7118=AXIS2_PLACEMENT_3D('',#18535,#8469,#8470);
#7119=AXIS2_PLACEMENT_3D('',#18537,#8471,#8472);
#7120=AXIS2_PLACEMENT_3D('',#18540,#8474,#8475);
#7121=AXIS2_PLACEMENT_3D('',#18541,#8476,#8477);
#7122=AXIS2_PLACEMENT_3D('',#18543,#8478,#8479);
#7123=AXIS2_PLACEMENT_3D('',#18546,#8481,#8482);
#7124=AXIS2_PLACEMENT_3D('',#18547,#8483,#8484);
#7125=AXIS2_PLACEMENT_3D('',#18548,#8485,#8486);
#7126=AXIS2_PLACEMENT_3D('',#18549,#8487,#8488);
#7127=AXIS2_PLACEMENT_3D('',#18550,#8489,#8490);
#7128=AXIS2_PLACEMENT_3D('',#18551,#8491,#8492);
#7129=AXIS2_PLACEMENT_3D('',#18552,#8493,#8494);
#7130=AXIS2_PLACEMENT_3D('',#18553,#8495,#8496);
#7131=AXIS2_PLACEMENT_3D('',#18554,#8497,#8498);
#7132=AXIS2_PLACEMENT_3D('',#18555,#8499,#8500);
#7133=AXIS2_PLACEMENT_3D('',#18556,#8501,#8502);
#7134=DIRECTION('axis',(0.,0.,1.));
#7135=DIRECTION('refdir',(1.,0.,0.));
#7136=DIRECTION('axis',(0.,0.,1.));
#7137=DIRECTION('refdir',(1.,0.,0.));
#7138=DIRECTION('center_axis',(0.,0.,-1.));
#7139=DIRECTION('ref_axis',(1.,0.,0.));
#7140=DIRECTION('center_axis',(0.,0.,-1.));
#7141=DIRECTION('ref_axis',(1.,0.,0.));
#7142=DIRECTION('',(0.,0.,-1.));
#7143=DIRECTION('center_axis',(0.,0.,1.));
#7144=DIRECTION('ref_axis',(1.,0.,0.));
#7145=DIRECTION('center_axis',(0.,0.,-1.));
#7146=DIRECTION('ref_axis',(1.,0.,0.));
#7147=DIRECTION('center_axis',(0.,0.,-1.));
#7148=DIRECTION('ref_axis',(1.,0.,0.));
#7149=DIRECTION('',(0.,0.,-1.));
#7150=DIRECTION('center_axis',(0.,0.,1.));
#7151=DIRECTION('ref_axis',(1.,0.,0.));
#7152=DIRECTION('center_axis',(0.,0.,-1.));
#7153=DIRECTION('ref_axis',(1.,0.,0.));
#7154=DIRECTION('center_axis',(0.,0.,-1.));
#7155=DIRECTION('ref_axis',(1.,0.,0.));
#7156=DIRECTION('',(0.,0.,-1.));
#7157=DIRECTION('center_axis',(0.,0.,1.));
#7158=DIRECTION('ref_axis',(1.,0.,0.));
#7159=DIRECTION('center_axis',(1.,0.,0.));
#7160=DIRECTION('ref_axis',(0.,0.,-1.));
#7161=DIRECTION('',(0.,-1.,0.));
#7162=DIRECTION('',(0.,0.832050294337844,0.554700196225229));
#7163=DIRECTION('',(0.,0.,1.));
#7164=DIRECTION('center_axis',(0.,0.554700196225229,-0.832050294337844));
#7165=DIRECTION('ref_axis',(0.,0.832050294337844,0.554700196225229));
#7166=DIRECTION('',(0.968400249412505,0.207514339159822,0.138342892773215));
#7167=DIRECTION('',(0.,0.832050294337844,0.554700196225229));
#7168=DIRECTION('',(-1.,0.,0.));
#7169=DIRECTION('',(1.,0.,0.));
#7170=DIRECTION('center_axis',(1.,0.,0.));
#7171=DIRECTION('ref_axis',(0.,2.22044604925031E-16,1.));
#7172=DIRECTION('',(0.,0.,-1.));
#7173=DIRECTION('',(0.,1.,0.));
#7174=DIRECTION('',(0.,0.,1.));
#7175=DIRECTION('center_axis',(0.,0.,1.));
#7176=DIRECTION('ref_axis',(1.,0.,0.));
#7177=DIRECTION('',(-0.97780241407741,-0.209529088730873,0.));
#7178=DIRECTION('',(0.707106781186546,-0.707106781186549,0.));
#7179=DIRECTION('center_axis',(0.,0.,1.));
#7180=DIRECTION('ref_axis',(1.,0.,0.));
#7181=DIRECTION('',(0.650791373455969,0.759256602365297,0.));
#7182=DIRECTION('',(0.,-1.,0.));
#7183=DIRECTION('',(-0.832050294337844,-0.554700196225229,0.));
#7184=DIRECTION('',(-0.993408935871131,-0.114624107985131,0.));
#7185=DIRECTION('',(-0.97780241407741,-0.209529088730873,0.));
#7186=DIRECTION('center_axis',(-0.554700196225229,0.832050294337844,0.));
#7187=DIRECTION('ref_axis',(-0.832050294337844,-0.554700196225229,0.));
#7188=DIRECTION('',(0.,0.,1.));
#7189=DIRECTION('',(0.832050294337844,0.554700196225229,0.));
#7190=DIRECTION('',(0.,0.,1.));
#7191=DIRECTION('center_axis',(0.759256602365297,-0.650791373455969,0.));
#7192=DIRECTION('ref_axis',(0.650791373455969,0.759256602365297,0.));
#7193=DIRECTION('',(0.,0.,-1.));
#7194=DIRECTION('',(-0.650791373455969,-0.759256602365297,0.));
#7195=DIRECTION('center_axis',(-0.707106781186549,-0.707106781186546,0.));
#7196=DIRECTION('ref_axis',(0.707106781186546,-0.707106781186549,0.));
#7197=DIRECTION('',(-0.707106781186546,0.707106781186549,0.));
#7198=DIRECTION('',(0.,0.,1.));
#7199=DIRECTION('center_axis',(-0.209529088730873,0.97780241407741,0.));
#7200=DIRECTION('ref_axis',(-0.97780241407741,-0.209529088730873,0.));
#7201=DIRECTION('',(0.,0.,1.));
#7202=DIRECTION('',(0.97780241407741,0.209529088730873,0.));
#7203=DIRECTION('center_axis',(-0.114624107985131,0.993408935871131,0.));
#7204=DIRECTION('ref_axis',(-0.993408935871131,-0.114624107985131,0.));
#7205=DIRECTION('',(0.993408935871131,0.114624107985131,0.));
#7206=DIRECTION('center_axis',(0.,0.,1.));
#7207=DIRECTION('ref_axis',(1.,0.,0.));
#7208=DIRECTION('',(0.,1.,0.));
#7209=DIRECTION('',(1.,0.,0.));
#7210=DIRECTION('',(0.,-1.,0.));
#7211=DIRECTION('center_axis',(0.,0.,1.));
#7212=DIRECTION('ref_axis',(1.,0.,0.));
#7213=DIRECTION('',(-0.447213595499958,-0.894427190999916,0.));
#7214=DIRECTION('',(-0.694594513699567,0.719401460617409,0.));
#7215=DIRECTION('',(-1.,0.,0.));
#7216=DIRECTION('',(0.,1.,0.));
#7217=DIRECTION('',(1.,0.,0.));
#7218=DIRECTION('',(0.87524153543927,-0.483686111690123,0.));
#7219=DIRECTION('center_axis',(0.,0.,1.));
#7220=DIRECTION('ref_axis',(1.,0.,0.));
#7221=DIRECTION('',(-1.,0.,0.));
#7222=DIRECTION('',(0.,1.,0.));
#7223=DIRECTION('center_axis',(0.,-1.,0.));
#7224=DIRECTION('ref_axis',(1.,0.,0.));
#7225=DIRECTION('',(0.,0.,-1.));
#7226=DIRECTION('',(1.,0.,0.));
#7227=DIRECTION('',(0.,0.,1.));
#7228=DIRECTION('center_axis',(-1.,0.,0.));
#7229=DIRECTION('ref_axis',(0.,-1.,0.));
#7230=DIRECTION('',(0.,-1.,0.));
#7231=DIRECTION('',(0.,0.,1.));
#7232=DIRECTION('center_axis',(0.,1.,0.));
#7233=DIRECTION('ref_axis',(-1.,0.,0.));
#7234=DIRECTION('',(-1.,0.,0.));
#7235=DIRECTION('',(0.,0.,1.));
#7236=DIRECTION('center_axis',(1.,0.,0.));
#7237=DIRECTION('ref_axis',(0.,1.,0.));
#7238=DIRECTION('',(0.,0.,1.));
#7239=DIRECTION('',(0.,1.,0.));
#7240=DIRECTION('center_axis',(0.,0.,1.));
#7241=DIRECTION('ref_axis',(1.,0.,0.));
#7242=DIRECTION('',(0.,0.,1.));
#7243=DIRECTION('center_axis',(0.,0.,1.));
#7244=DIRECTION('ref_axis',(1.,0.,0.));
#7245=DIRECTION('center_axis',(0.,0.,1.));
#7246=DIRECTION('ref_axis',(1.,0.,0.));
#7247=DIRECTION('center_axis',(0.,0.,1.));
#7248=DIRECTION('ref_axis',(1.,0.,0.));
#7249=DIRECTION('',(0.,0.,-1.));
#7250=DIRECTION('center_axis',(0.,0.,1.));
#7251=DIRECTION('ref_axis',(1.,0.,0.));
#7252=DIRECTION('',(0.87524153543927,-0.483686111690123,0.));
#7253=DIRECTION('',(1.,0.,0.));
#7254=DIRECTION('',(0.,1.,0.));
#7255=DIRECTION('',(-1.,0.,0.));
#7256=DIRECTION('',(-0.694594513699567,0.719401460617409,0.));
#7257=DIRECTION('',(-0.447213595499958,-0.894427190999916,0.));
#7258=DIRECTION('center_axis',(-0.483686111690123,-0.87524153543927,0.));
#7259=DIRECTION('ref_axis',(0.87524153543927,-0.483686111690123,0.));
#7260=DIRECTION('',(0.,0.,1.));
#7261=DIRECTION('center_axis',(-0.894427190999916,0.447213595499958,0.));
#7262=DIRECTION('ref_axis',(-0.447213595499958,-0.894427190999916,0.));
#7263=DIRECTION('',(0.,0.,1.));
#7264=DIRECTION('center_axis',(0.719401460617409,0.694594513699567,0.));
#7265=DIRECTION('ref_axis',(-0.694594513699567,0.719401460617409,0.));
#7266=DIRECTION('',(0.,0.,1.));
#7267=DIRECTION('center_axis',(0.,1.,0.));
#7268=DIRECTION('ref_axis',(-1.,0.,0.));
#7269=DIRECTION('',(0.,0.,1.));
#7270=DIRECTION('center_axis',(1.,0.,0.));
#7271=DIRECTION('ref_axis',(0.,1.,0.));
#7272=DIRECTION('',(0.,0.,1.));
#7273=DIRECTION('center_axis',(0.,-1.,0.));
#7274=DIRECTION('ref_axis',(1.,0.,0.));
#7275=DIRECTION('axis',(0.,0.,1.));
#7276=DIRECTION('refdir',(1.,0.,0.));
#7277=DIRECTION('center_axis',(0.,0.,1.));
#7278=DIRECTION('ref_axis',(1.,0.,0.));
#7279=DIRECTION('center_axis',(0.,0.,1.));
#7280=DIRECTION('ref_axis',(1.,0.,0.));
#7281=DIRECTION('',(0.,0.,1.));
#7282=DIRECTION('center_axis',(0.,0.,1.));
#7283=DIRECTION('ref_axis',(1.,0.,0.));
#7284=DIRECTION('center_axis',(0.,0.,-1.));
#7285=DIRECTION('ref_axis',(-1.,0.,0.));
#7286=DIRECTION('center_axis',(0.,0.,-1.));
#7287=DIRECTION('ref_axis',(1.,0.,0.));
#7288=DIRECTION('center_axis',(0.,0.,1.));
#7289=DIRECTION('ref_axis',(1.,0.,0.));
#7290=DIRECTION('center_axis',(0.,0.,1.));
#7291=DIRECTION('ref_axis',(1.,0.,0.));
#7292=DIRECTION('center_axis',(0.,0.,1.));
#7293=DIRECTION('ref_axis',(1.,0.,0.));
#7294=DIRECTION('center_axis',(0.,0.,1.));
#7295=DIRECTION('ref_axis',(1.,0.,0.));
#7296=DIRECTION('',(0.,0.,-1.));
#7297=DIRECTION('center_axis',(0.,0.,1.));
#7298=DIRECTION('ref_axis',(1.,0.,0.));
#7299=DIRECTION('center_axis',(0.,0.,1.));
#7300=DIRECTION('ref_axis',(1.,0.,0.));
#7301=DIRECTION('center_axis',(0.,0.,1.));
#7302=DIRECTION('ref_axis',(1.,0.,0.));
#7303=DIRECTION('center_axis',(0.,0.,1.));
#7304=DIRECTION('ref_axis',(1.,0.,0.));
#7305=DIRECTION('',(0.,0.,-1.));
#7306=DIRECTION('center_axis',(0.,0.,1.));
#7307=DIRECTION('ref_axis',(1.,0.,0.));
#7308=DIRECTION('center_axis',(0.,0.,1.));
#7309=DIRECTION('ref_axis',(1.,0.,0.));
#7310=DIRECTION('center_axis',(0.,0.,1.));
#7311=DIRECTION('ref_axis',(1.,0.,0.));
#7312=DIRECTION('',(0.,0.,-1.));
#7313=DIRECTION('center_axis',(0.,0.,1.));
#7314=DIRECTION('ref_axis',(1.,0.,0.));
#7315=DIRECTION('axis',(0.,0.,1.));
#7316=DIRECTION('refdir',(1.,0.,0.));
#7317=DIRECTION('center_axis',(-1.,0.,0.));
#7318=DIRECTION('ref_axis',(0.,1.,0.));
#7319=DIRECTION('',(0.,0.,1.));
#7320=DIRECTION('',(0.,-1.,0.));
#7321=DIRECTION('',(0.,0.,-1.));
#7322=DIRECTION('',(0.,1.,0.));
#7323=DIRECTION('center_axis',(1.,0.,0.));
#7324=DIRECTION('ref_axis',(0.,-1.,0.));
#7325=DIRECTION('',(0.,0.,-1.));
#7326=DIRECTION('',(0.,-1.,0.));
#7327=DIRECTION('',(0.,0.,1.));
#7328=DIRECTION('',(0.,1.,0.));
#7329=DIRECTION('center_axis',(0.,0.,1.));
#7330=DIRECTION('ref_axis',(1.,0.,0.));
#7331=DIRECTION('center_axis',(0.,0.,1.));
#7332=DIRECTION('ref_axis',(1.,0.,0.));
#7333=DIRECTION('center_axis',(0.,0.,-1.));
#7334=DIRECTION('ref_axis',(1.,0.,0.));
#7335=DIRECTION('center_axis',(0.,0.,1.));
#7336=DIRECTION('ref_axis',(6.12323399573677E-17,-1.,0.));
#7337=DIRECTION('center_axis',(0.,0.,-1.));
#7338=DIRECTION('ref_axis',(1.,0.,0.));
#7339=DIRECTION('center_axis',(0.,0.,1.));
#7340=DIRECTION('ref_axis',(6.12323399573677E-17,-1.,0.));
#7341=DIRECTION('center_axis',(0.,0.,1.));
#7342=DIRECTION('ref_axis',(1.,0.,0.));
#7343=DIRECTION('center_axis',(0.,0.,1.));
#7344=DIRECTION('ref_axis',(1.,0.,0.));
#7345=DIRECTION('axis',(0.,0.,1.));
#7346=DIRECTION('refdir',(1.,0.,0.));
#7347=DIRECTION('axis',(0.,0.,1.));
#7348=DIRECTION('refdir',(1.,0.,0.));
#7349=DIRECTION('center_axis',(0.,0.,-1.));
#7350=DIRECTION('ref_axis',(1.,0.,0.));
#7351=DIRECTION('center_axis',(0.,0.,1.));
#7352=DIRECTION('ref_axis',(1.,0.,0.));
#7353=DIRECTION('center_axis',(0.,0.,-1.));
#7354=DIRECTION('ref_axis',(1.,0.,0.));
#7355=DIRECTION('center_axis',(0.,0.,1.));
#7356=DIRECTION('ref_axis',(1.,0.,0.));
#7357=DIRECTION('center_axis',(0.,0.,-1.));
#7358=DIRECTION('ref_axis',(1.,0.,0.));
#7359=DIRECTION('center_axis',(0.,0.,1.));
#7360=DIRECTION('ref_axis',(1.,0.,0.));
#7361=DIRECTION('center_axis',(0.,0.,-1.));
#7362=DIRECTION('ref_axis',(1.,0.,0.));
#7363=DIRECTION('center_axis',(0.,0.,1.));
#7364=DIRECTION('ref_axis',(1.,0.,0.));
#7365=DIRECTION('center_axis',(4.10828654779316E-33,-1.13946463231163E-19,
1.));
#7366=DIRECTION('ref_axis',(1.,0.,-4.10828654779316E-33));
#7367=DIRECTION('',(0.,1.,1.13946463231163E-19));
#7368=DIRECTION('',(0.,-1.,-1.13946463231163E-19));
#7369=DIRECTION('center_axis',(4.10828654779316E-33,-1.13946463231163E-19,
1.));
#7370=DIRECTION('ref_axis',(1.,0.,0.));
#7371=DIRECTION('center_axis',(4.10828654779316E-33,-1.13946463231163E-19,
1.));
#7372=DIRECTION('ref_axis',(1.,0.,0.));
#7373=DIRECTION('center_axis',(4.10828654779316E-33,-1.13946463231163E-19,
1.));
#7374=DIRECTION('ref_axis',(1.,0.,0.));
#7375=DIRECTION('center_axis',(0.,0.,-1.));
#7376=DIRECTION('ref_axis',(1.,0.,0.));
#7377=DIRECTION('center_axis',(-4.10828654779316E-33,1.13946463231163E-19,
-1.));
#7378=DIRECTION('ref_axis',(1.,0.,0.));
#7379=DIRECTION('',(0.,0.,-1.));
#7380=DIRECTION('center_axis',(0.,0.,-1.));
#7381=DIRECTION('ref_axis',(1.,0.,0.));
#7382=DIRECTION('center_axis',(-4.10828654779316E-33,1.13946463231163E-19,
-1.));
#7383=DIRECTION('ref_axis',(1.,0.,0.));
#7384=DIRECTION('',(0.,0.,-1.));
#7385=DIRECTION('center_axis',(4.10828654779316E-33,-1.13946463231163E-19,
1.));
#7386=DIRECTION('ref_axis',(1.,0.,0.));
#7387=DIRECTION('center_axis',(0.,0.,-1.));
#7388=DIRECTION('ref_axis',(1.,0.,0.));
#7389=DIRECTION('center_axis',(-4.10828654779316E-33,1.13946463231163E-19,
-1.));
#7390=DIRECTION('ref_axis',(1.,0.,0.));
#7391=DIRECTION('',(0.,0.,-1.));
#7392=DIRECTION('center_axis',(4.10828654779316E-33,-1.13946463231163E-19,
1.));
#7393=DIRECTION('ref_axis',(1.,0.,0.));
#7394=DIRECTION('center_axis',(0.,0.,-1.));
#7395=DIRECTION('ref_axis',(1.,0.,0.));
#7396=DIRECTION('center_axis',(-4.10828654779316E-33,1.13946463231163E-19,
-1.));
#7397=DIRECTION('ref_axis',(1.,0.,0.));
#7398=DIRECTION('',(0.,0.,-1.));
#7399=DIRECTION('center_axis',(0.,0.,-1.));
#7400=DIRECTION('ref_axis',(1.,0.,0.));
#7401=DIRECTION('center_axis',(-4.10828654779316E-33,1.13946463231163E-19,
-1.));
#7402=DIRECTION('ref_axis',(1.,0.,0.));
#7403=DIRECTION('',(0.,0.,-1.));
#7404=DIRECTION('center_axis',(0.,0.,-1.));
#7405=DIRECTION('ref_axis',(1.,0.,0.));
#7406=DIRECTION('center_axis',(0.,0.,-1.));
#7407=DIRECTION('ref_axis',(1.,0.,0.));
#7408=DIRECTION('center_axis',(0.,0.,1.));
#7409=DIRECTION('ref_axis',(1.,0.,0.));
#7410=DIRECTION('center_axis',(0.,0.,-1.));
#7411=DIRECTION('ref_axis',(1.,0.,0.));
#7412=DIRECTION('center_axis',(-4.10828654779316E-33,1.13946463231163E-19,
-1.));
#7413=DIRECTION('ref_axis',(1.,0.,0.));
#7414=DIRECTION('',(0.,0.,-1.));
#7415=DIRECTION('center_axis',(0.,0.,-1.));
#7416=DIRECTION('ref_axis',(1.,0.,0.));
#7417=DIRECTION('center_axis',(0.,0.,-1.));
#7418=DIRECTION('ref_axis',(1.,0.,0.));
#7419=DIRECTION('center_axis',(0.,0.,1.));
#7420=DIRECTION('ref_axis',(1.,0.,0.));
#7421=DIRECTION('center_axis',(0.,0.,-1.));
#7422=DIRECTION('ref_axis',(1.,0.,0.));
#7423=DIRECTION('',(0.,0.,-1.));
#7424=DIRECTION('center_axis',(0.,0.,1.));
#7425=DIRECTION('ref_axis',(1.,0.,0.));
#7426=DIRECTION('center_axis',(0.,0.,-1.));
#7427=DIRECTION('ref_axis',(1.,0.,0.));
#7428=DIRECTION('',(0.,0.,-1.));
#7429=DIRECTION('center_axis',(0.,0.,1.));
#7430=DIRECTION('ref_axis',(1.,0.,0.));
#7431=DIRECTION('center_axis',(0.,-1.,0.));
#7432=DIRECTION('ref_axis',(-1.,0.,0.));
#7433=DIRECTION('',(0.0523359562429438,0.,0.998629534754574));
#7434=DIRECTION('',(1.,0.,0.));
#7435=DIRECTION('',(-0.0523359562429438,0.,-0.998629534754574));
#7436=DIRECTION('',(1.,0.,0.));
#7437=DIRECTION('center_axis',(0.,-1.,0.));
#7438=DIRECTION('ref_axis',(-1.,0.,0.));
#7439=DIRECTION('',(0.,0.,-1.));
#7440=DIRECTION('',(1.,0.,0.));
#7441=DIRECTION('',(0.,0.,1.));
#7442=DIRECTION('',(1.,0.,0.));
#7443=DIRECTION('center_axis',(0.,-1.,0.));
#7444=DIRECTION('ref_axis',(-1.,0.,0.));
#7445=DIRECTION('',(0.,0.,-1.));
#7446=DIRECTION('',(1.,0.,0.));
#7447=DIRECTION('',(0.,0.,1.));
#7448=DIRECTION('',(1.,0.,0.));
#7449=DIRECTION('center_axis',(0.,-1.,0.));
#7450=DIRECTION('ref_axis',(-1.,0.,0.));
#7451=DIRECTION('',(0.,0.,-1.));
#7452=DIRECTION('',(1.,0.,0.));
#7453=DIRECTION('',(0.,0.,1.));
#7454=DIRECTION('',(1.,0.,0.));
#7455=DIRECTION('center_axis',(0.,1.,0.));
#7456=DIRECTION('ref_axis',(1.,0.,0.));
#7457=DIRECTION('',(-0.0523359562429438,0.,-0.998629534754574));
#7458=DIRECTION('',(-1.,0.,0.));
#7459=DIRECTION('',(0.0523359562429438,0.,0.998629534754574));
#7460=DIRECTION('',(-1.,0.,0.));
#7461=DIRECTION('center_axis',(0.,1.,0.));
#7462=DIRECTION('ref_axis',(1.,0.,0.));
#7463=DIRECTION('',(0.,0.,1.));
#7464=DIRECTION('',(-1.,0.,0.));
#7465=DIRECTION('',(0.,0.,-1.));
#7466=DIRECTION('',(-1.,0.,0.));
#7467=DIRECTION('center_axis',(0.,1.,0.));
#7468=DIRECTION('ref_axis',(1.,0.,0.));
#7469=DIRECTION('',(0.,0.,1.));
#7470=DIRECTION('',(-1.,0.,0.));
#7471=DIRECTION('',(0.,0.,-1.));
#7472=DIRECTION('',(-1.,0.,0.));
#7473=DIRECTION('center_axis',(0.,0.,1.));
#7474=DIRECTION('ref_axis',(1.,0.,0.));
#7475=DIRECTION('center_axis',(0.,0.,1.));
#7476=DIRECTION('ref_axis',(1.,0.,0.));
#7477=DIRECTION('center_axis',(0.,0.,1.));
#7478=DIRECTION('ref_axis',(1.,0.,0.));
#7479=DIRECTION('center_axis',(0.,0.,1.));
#7480=DIRECTION('ref_axis',(1.,0.,0.));
#7481=DIRECTION('center_axis',(0.,0.,1.));
#7482=DIRECTION('ref_axis',(1.,0.,0.));
#7483=DIRECTION('',(0.,1.,0.));
#7484=DIRECTION('',(0.,-1.,0.));
#7485=DIRECTION('center_axis',(0.,0.,1.));
#7486=DIRECTION('ref_axis',(1.,0.,0.));
#7487=DIRECTION('',(0.,-1.,0.));
#7488=DIRECTION('',(0.,1.,0.));
#7489=DIRECTION('center_axis',(0.,0.,1.));
#7490=DIRECTION('ref_axis',(1.,0.,0.));
#7491=DIRECTION('',(0.,-1.,0.));
#7492=DIRECTION('',(0.,1.,0.));
#7493=DIRECTION('center_axis',(0.,0.,1.));
#7494=DIRECTION('ref_axis',(1.,0.,0.));
#7495=DIRECTION('',(0.,-1.,0.));
#7496=DIRECTION('',(-1.,0.,0.));
#7497=DIRECTION('',(0.,1.,0.));
#7498=DIRECTION('center_axis',(0.,1.,0.));
#7499=DIRECTION('ref_axis',(1.,0.,0.));
#7500=DIRECTION('',(0.,0.,1.));
#7501=DIRECTION('',(-1.,0.,0.));
#7502=DIRECTION('',(0.,0.,-1.));
#7503=DIRECTION('center_axis',(-1.,0.,0.));
#7504=DIRECTION('ref_axis',(0.,-1.,0.));
#7505=DIRECTION('',(0.,-1.,0.));
#7506=DIRECTION('center_axis',(1.,0.,0.));
#7507=DIRECTION('ref_axis',(0.,1.,0.));
#7508=DIRECTION('',(0.,1.,0.));
#7509=DIRECTION('',(0.,1.,0.));
#7510=DIRECTION('center_axis',(1.,0.,0.));
#7511=DIRECTION('ref_axis',(0.,1.,0.));
#7512=DIRECTION('',(0.,1.,0.));
#7513=DIRECTION('',(0.,1.,1.13946463231163E-19));
#7514=DIRECTION('',(0.,1.,0.));
#7515=DIRECTION('center_axis',(1.,0.,0.));
#7516=DIRECTION('ref_axis',(0.,1.,0.));
#7517=DIRECTION('',(0.,1.,0.));
#7518=DIRECTION('',(0.,1.,1.13946463231163E-19));
#7519=DIRECTION('',(0.,1.,0.));
#7520=DIRECTION('center_axis',(0.998629534754574,0.,-0.0523359562429438));
#7521=DIRECTION('ref_axis',(-0.0523359562429438,0.,-0.998629534754574));
#7522=DIRECTION('',(0.,-1.,0.));
#7523=DIRECTION('',(-5.97168109510197E-21,-1.,-1.13946463231163E-19));
#7524=DIRECTION('',(0.,-1.,0.));
#7525=DIRECTION('center_axis',(0.,0.,1.));
#7526=DIRECTION('ref_axis',(1.,0.,0.));
#7527=DIRECTION('',(0.,-1.,0.));
#7528=DIRECTION('',(0.,-1.,0.));
#7529=DIRECTION('',(0.,-1.,0.));
#7530=DIRECTION('',(0.,1.,0.));
#7531=DIRECTION('',(0.,-1.,0.));
#7532=DIRECTION('',(0.,1.,0.));
#7533=DIRECTION('',(0.,-1.,0.));
#7534=DIRECTION('',(0.,-1.,0.));
#7535=DIRECTION('',(0.,-1.,0.));
#7536=DIRECTION('',(0.,1.,0.));
#7537=DIRECTION('',(0.,1.,0.));
#7538=DIRECTION('center_axis',(0.,0.,1.));
#7539=DIRECTION('ref_axis',(1.,0.,0.));
#7540=DIRECTION('',(0.,0.,-1.));
#7541=DIRECTION('center_axis',(0.,0.,1.));
#7542=DIRECTION('ref_axis',(1.,0.,0.));
#7543=DIRECTION('center_axis',(4.10828654779316E-33,-1.13946463231163E-19,
1.));
#7544=DIRECTION('ref_axis',(1.,0.,0.));
#7545=DIRECTION('',(0.,0.,-1.));
#7546=DIRECTION('center_axis',(1.,0.,0.));
#7547=DIRECTION('ref_axis',(0.,1.,0.));
#7548=DIRECTION('',(0.,1.,1.13946463231163E-19));
#7549=DIRECTION('center_axis',(0.99852593895705,0.0542765992849681,9.38276897523041E-9));
#7550=DIRECTION('ref_axis',(0.0541946171271057,-0.99701772369063,0.0549418066794405));
#7551=DIRECTION('center_axis',(4.10828654779316E-33,-1.13946463231163E-19,
1.));
#7552=DIRECTION('ref_axis',(1.,0.,-4.10828654779316E-33));
#7553=DIRECTION('',(5.97168109510217E-21,-1.,-1.13946463231163E-19));
#7554=DIRECTION('center_axis',(-1.,0.,0.));
#7555=DIRECTION('ref_axis',(0.,-1.,0.));
#7556=DIRECTION('',(0.,-1.,-1.13946463231163E-19));
#7557=DIRECTION('center_axis',(4.10828654779316E-33,-1.13946463231163E-19,
1.));
#7558=DIRECTION('ref_axis',(1.,0.,-4.10828654779316E-33));
#7559=DIRECTION('center_axis',(-1.,0.,0.));
#7560=DIRECTION('ref_axis',(0.,-1.,0.));
#7561=DIRECTION('',(0.,-1.,-1.13946463231163E-19));
#7562=DIRECTION('center_axis',(4.10828654779316E-33,-1.13946463231163E-19,
1.));
#7563=DIRECTION('ref_axis',(1.,0.,-4.10828654779316E-33));
#7564=DIRECTION('center_axis',(-1.,0.,0.));
#7565=DIRECTION('ref_axis',(0.,-1.,0.));
#7566=DIRECTION('',(0.,-1.,-1.13946463231163E-19));
#7567=DIRECTION('center_axis',(-0.996961060527779,0.0779015005717205,0.));
#7568=DIRECTION('ref_axis',(0.,0.,1.));
#7569=DIRECTION('center_axis',(4.10828654779316E-33,-1.13946463231163E-19,
1.));
#7570=DIRECTION('ref_axis',(1.,0.,-4.10828654779316E-33));
#7571=DIRECTION('',(5.97168109510197E-21,1.,1.13946463231163E-19));
#7572=DIRECTION('center_axis',(-0.996961060527779,-0.0779015005717276,-4.485055189269E-15));
#7573=DIRECTION('ref_axis',(-0.0777791112471086,0.995394757055134,0.0560329142626144));
#7574=DIRECTION('center_axis',(-0.377317868652411,-0.840644185582845,0.388521015186253));
#7575=DIRECTION('ref_axis',(-0.58566693710526,0.541587807512093,0.603056287203763));
#7576=DIRECTION('center_axis',(7.41164423166535E-16,1.,0.));
#7577=DIRECTION('ref_axis',(0.,0.,1.));
#7578=DIRECTION('center_axis',(0.0522650005536027,-0.0520548592672972,0.997275619547472));
#7579=DIRECTION('ref_axis',(-0.998629534754574,7.40148683083438E-16,0.0523359562429445));
#7580=DIRECTION('center_axis',(0.376559988603802,-0.837471124372148,0.396036224133039));
#7581=DIRECTION('ref_axis',(0.577069986161316,0.546481578685729,0.606916893181374));
#7582=DIRECTION('center_axis',(0.998525938475037,-0.0542766081525538,0.));
#7583=DIRECTION('ref_axis',(0.,0.,1.));
#7584=DIRECTION('center_axis',(-0.0522648366634829,-0.0521149007022807,
0.997272492337641));
#7585=DIRECTION('ref_axis',(0.0541946171271058,0.99701772369063,0.0549418066794413));
#7586=DIRECTION('center_axis',(5.32220538281047E-11,1.,-1.01553728389566E-9));
#7587=DIRECTION('ref_axis',(0.998629534754574,0.,0.0523359562429456));
#7588=DIRECTION('center_axis',(0.37731786865241,-0.840644185582843,-0.388521015186259));
#7589=DIRECTION('ref_axis',(-0.585666937105255,-0.541587807512096,0.603056287203765));
#7590=DIRECTION('center_axis',(0.0522650005536027,0.0520548592672965,0.997275619547472));
#7591=DIRECTION('ref_axis',(-0.0777791112471059,-0.995394757055134,0.0560329142626137));
#7592=DIRECTION('center_axis',(0.,-1.,0.));
#7593=DIRECTION('ref_axis',(-0.998629534754574,0.,0.0523359562429439));
#7594=DIRECTION('center_axis',(5.97168109510197E-21,1.,1.13946463231163E-19));
#7595=DIRECTION('ref_axis',(-0.688354575693753,0.,0.725374371012288));
#7596=DIRECTION('center_axis',(-0.376559987018669,-0.837471124206646,-0.396036225990193));
#7597=DIRECTION('ref_axis',(0.577069983350267,-0.54648157893936,0.606916895625808));
#7598=DIRECTION('center_axis',(-0.0522648366634817,0.0521149007022785,0.997272492337641));
#7599=DIRECTION('ref_axis',(0.998629534754574,0.,0.052335956242946));
#7600=DIRECTION('center_axis',(1.01693095242295E-9,-1.,0.));
#7601=DIRECTION('ref_axis',(0.,0.,1.));
#7602=DIRECTION('center_axis',(5.97168109510217E-21,-1.,-1.13946463231163E-19));
#7603=DIRECTION('ref_axis',(0.688354575693753,0.,0.725374371012289));
#7604=DIRECTION('',(-5.97168109510217E-21,1.,1.13946463231163E-19));
#7605=DIRECTION('center_axis',(-0.998629534754574,0.,-0.0523359562429455));
#7606=DIRECTION('ref_axis',(-0.0523359562429455,0.,0.998629534754574));
#7607=DIRECTION('center_axis',(-0.377317868652411,-0.840644185582845,0.388521015186254));
#7608=DIRECTION('ref_axis',(-0.585666937105261,0.541587807512092,0.603056287203763));
#7609=DIRECTION('center_axis',(7.41164423166535E-16,1.,0.));
#7610=DIRECTION('ref_axis',(0.,0.,1.));
#7611=DIRECTION('center_axis',(-0.996961060527779,-0.0779015005717276,-4.485055189269E-15));
#7612=DIRECTION('ref_axis',(-0.0777791112471086,0.995394757055134,0.0560329142626144));
#7613=DIRECTION('center_axis',(0.0522650005536027,-0.0520548592672972,0.997275619547472));
#7614=DIRECTION('ref_axis',(-0.998629534754574,7.40148683083438E-16,0.0523359562429445));
#7615=DIRECTION('center_axis',(0.376559988603802,-0.837471124372148,0.396036224133039));
#7616=DIRECTION('ref_axis',(0.577069986161311,0.546481578685732,0.606916893181376));
#7617=DIRECTION('center_axis',(0.998525938475037,-0.0542766081525538,0.));
#7618=DIRECTION('ref_axis',(0.,0.,1.));
#7619=DIRECTION('center_axis',(5.32220538281047E-11,1.,-1.01553728389566E-9));
#7620=DIRECTION('ref_axis',(0.998629534754574,0.,0.0523359562429456));
#7621=DIRECTION('center_axis',(-0.0522648366634829,-0.0521149007022807,
0.997272492337641));
#7622=DIRECTION('ref_axis',(0.0541946171271058,0.99701772369063,0.0549418066794413));
#7623=DIRECTION('center_axis',(0.37731786865241,-0.840644185582843,-0.388521015186259));
#7624=DIRECTION('ref_axis',(-0.585666937105255,-0.541587807512095,0.603056287203766));
#7625=DIRECTION('center_axis',(-0.996961060527779,0.0779015005717205,0.));
#7626=DIRECTION('ref_axis',(0.,0.,1.));
#7627=DIRECTION('center_axis',(0.,-1.,0.));
#7628=DIRECTION('ref_axis',(-0.998629534754574,0.,0.0523359562429439));
#7629=DIRECTION('center_axis',(0.0522650005536027,0.0520548592672965,0.997275619547472));
#7630=DIRECTION('ref_axis',(-0.0777791112471059,-0.995394757055134,0.0560329142626137));
#7631=DIRECTION('center_axis',(5.97168109510197E-21,1.,1.13946463231163E-19));
#7632=DIRECTION('ref_axis',(-0.688354575693753,0.,0.725374371012289));
#7633=DIRECTION('',(-5.97168109510197E-21,-1.,-1.13946463231163E-19));
#7634=DIRECTION('',(5.97168109510197E-21,1.,1.13946463231163E-19));
#7635=DIRECTION('center_axis',(-0.376559987018669,-0.837471124206646,-0.396036225990194));
#7636=DIRECTION('ref_axis',(0.577069983350267,-0.546481578939359,0.606916895625808));
#7637=DIRECTION('center_axis',(-0.0522648366634817,0.0521149007022785,0.997272492337641));
#7638=DIRECTION('ref_axis',(0.998629534754574,0.,0.052335956242946));
#7639=DIRECTION('center_axis',(1.01693095242295E-9,-1.,0.));
#7640=DIRECTION('ref_axis',(0.,0.,1.));
#7641=DIRECTION('center_axis',(0.99852593895705,0.0542765992849681,9.38276897523041E-9));
#7642=DIRECTION('ref_axis',(0.0541946171271057,-0.99701772369063,0.0549418066794405));
#7643=DIRECTION('center_axis',(5.97168109510217E-21,-1.,-1.13946463231163E-19));
#7644=DIRECTION('ref_axis',(0.688354575693753,0.,0.725374371012289));
#7645=DIRECTION('',(-5.97168109510217E-21,1.,1.13946463231163E-19));
#7646=DIRECTION('',(5.97168109510217E-21,-1.,-1.13946463231163E-19));
#7647=DIRECTION('center_axis',(0.998629534754574,0.,-0.0523359562429438));
#7648=DIRECTION('ref_axis',(-0.0523359562429438,0.,-0.998629534754574));
#7649=DIRECTION('center_axis',(4.10828654779316E-33,-1.13946463231163E-19,
1.));
#7650=DIRECTION('ref_axis',(1.,0.,-4.10828654779316E-33));
#7651=DIRECTION('center_axis',(-0.998629534754574,0.,-0.0523359562429455));
#7652=DIRECTION('ref_axis',(-0.0523359562429455,0.,0.998629534754574));
#7653=DIRECTION('axis',(0.,0.,1.));
#7654=DIRECTION('refdir',(1.,0.,0.));
#7655=DIRECTION('center_axis',(0.,0.,-1.));
#7656=DIRECTION('ref_axis',(1.,0.,0.));
#7657=DIRECTION('center_axis',(0.,0.,1.));
#7658=DIRECTION('ref_axis',(1.,0.,0.));
#7659=DIRECTION('center_axis',(0.,0.,-1.));
#7660=DIRECTION('ref_axis',(1.,0.,0.));
#7661=DIRECTION('center_axis',(0.,0.,1.));
#7662=DIRECTION('ref_axis',(1.,0.,0.));
#7663=DIRECTION('center_axis',(0.,0.,-1.));
#7664=DIRECTION('ref_axis',(1.,0.,0.));
#7665=DIRECTION('center_axis',(0.,0.,1.));
#7666=DIRECTION('ref_axis',(1.,0.,0.));
#7667=DIRECTION('center_axis',(0.,0.,-1.));
#7668=DIRECTION('ref_axis',(1.,0.,0.));
#7669=DIRECTION('center_axis',(0.,0.,1.));
#7670=DIRECTION('ref_axis',(1.,0.,0.));
#7671=DIRECTION('center_axis',(4.10828654779316E-33,-1.13946463231163E-19,
1.));
#7672=DIRECTION('ref_axis',(1.,0.,-4.10828654779316E-33));
#7673=DIRECTION('',(0.,1.,1.13946463231163E-19));
#7674=DIRECTION('',(0.,-1.,-1.13946463231163E-19));
#7675=DIRECTION('center_axis',(4.10828654779316E-33,-1.13946463231163E-19,
1.));
#7676=DIRECTION('ref_axis',(1.,0.,0.));
#7677=DIRECTION('center_axis',(4.10828654779316E-33,-1.13946463231163E-19,
1.));
#7678=DIRECTION('ref_axis',(1.,0.,0.));
#7679=DIRECTION('center_axis',(4.10828654779316E-33,-1.13946463231163E-19,
1.));
#7680=DIRECTION('ref_axis',(1.,0.,0.));
#7681=DIRECTION('center_axis',(0.86602540378444,0.499999999999998,0.));
#7682=DIRECTION('ref_axis',(0.499999999999998,-0.86602540378444,0.));
#7683=DIRECTION('',(0.499999999999998,-0.86602540378444,-9.86805318295791E-20));
#7684=DIRECTION('',(0.,0.,-1.));
#7685=DIRECTION('',(0.499999999999998,-0.86602540378444,0.));
#7686=DIRECTION('',(0.,0.,-1.));
#7687=DIRECTION('center_axis',(1.60246890531964E-16,1.,0.));
#7688=DIRECTION('ref_axis',(1.,-1.60246890531964E-16,0.));
#7689=DIRECTION('',(1.,-1.60246890531964E-16,-4.12654611421307E-33));
#7690=DIRECTION('',(0.,0.,-1.));
#7691=DIRECTION('',(1.,-1.60246890531964E-16,0.));
#7692=DIRECTION('center_axis',(-0.86602540378444,0.499999999999998,0.));
#7693=DIRECTION('ref_axis',(0.499999999999998,0.86602540378444,0.));
#7694=DIRECTION('',(0.499999999999998,0.86602540378444,9.86805318295749E-20));
#7695=DIRECTION('',(0.,0.,-1.));
#7696=DIRECTION('',(0.499999999999998,0.86602540378444,0.));
#7697=DIRECTION('center_axis',(-0.86602540378444,-0.499999999999998,0.));
#7698=DIRECTION('ref_axis',(-0.499999999999998,0.86602540378444,0.));
#7699=DIRECTION('',(-0.499999999999998,0.86602540378444,9.86805318295791E-20));
#7700=DIRECTION('',(0.,0.,-1.));
#7701=DIRECTION('',(-0.499999999999998,0.86602540378444,0.));
#7702=DIRECTION('center_axis',(-1.60246890531964E-16,-1.,0.));
#7703=DIRECTION('ref_axis',(-1.,1.60246890531964E-16,0.));
#7704=DIRECTION('',(-1.,1.60246890531964E-16,4.12654611421307E-33));
#7705=DIRECTION('',(0.,0.,-1.));
#7706=DIRECTION('',(-1.,1.60246890531964E-16,0.));
#7707=DIRECTION('center_axis',(0.86602540378444,-0.499999999999998,0.));
#7708=DIRECTION('ref_axis',(-0.499999999999998,-0.86602540378444,0.));
#7709=DIRECTION('',(-0.499999999999998,-0.86602540378444,-9.86805318295749E-20));
#7710=DIRECTION('',(-0.499999999999998,-0.86602540378444,0.));
#7711=DIRECTION('center_axis',(0.,0.,-1.));
#7712=DIRECTION('ref_axis',(-1.,0.,0.));
#7713=DIRECTION('center_axis',(0.,0.,1.));
#7714=DIRECTION('ref_axis',(1.,0.,0.));
#7715=DIRECTION('center_axis',(0.866025403784439,0.5,0.));
#7716=DIRECTION('ref_axis',(0.5,-0.866025403784439,0.));
#7717=DIRECTION('',(0.5,-0.866025403784439,-9.86805318295789E-20));
#7718=DIRECTION('',(0.,0.,-1.));
#7719=DIRECTION('',(0.5,-0.866025403784439,0.));
#7720=DIRECTION('',(0.,0.,-1.));
#7721=DIRECTION('center_axis',(1.60246890531964E-16,1.,0.));
#7722=DIRECTION('ref_axis',(1.,-1.60246890531964E-16,0.));
#7723=DIRECTION('',(1.,-1.60246890531964E-16,-4.12654611421307E-33));
#7724=DIRECTION('',(0.,0.,-1.));
#7725=DIRECTION('',(1.,-1.60246890531964E-16,0.));
#7726=DIRECTION('center_axis',(-0.866025403784438,0.5,0.));
#7727=DIRECTION('ref_axis',(0.5,0.866025403784438,0.));
#7728=DIRECTION('',(0.5,0.866025403784438,9.86805318295748E-20));
#7729=DIRECTION('',(0.,0.,-1.));
#7730=DIRECTION('',(0.5,0.866025403784438,0.));
#7731=DIRECTION('center_axis',(-0.866025403784439,-0.499999999999999,0.));
#7732=DIRECTION('ref_axis',(-0.499999999999999,0.866025403784439,0.));
#7733=DIRECTION('',(-0.499999999999999,0.866025403784439,9.8680531829579E-20));
#7734=DIRECTION('',(0.,0.,-1.));
#7735=DIRECTION('',(-0.499999999999999,0.866025403784439,0.));
#7736=DIRECTION('center_axis',(-1.60246890531964E-16,-1.,0.));
#7737=DIRECTION('ref_axis',(-1.,1.60246890531964E-16,0.));
#7738=DIRECTION('',(-1.,1.60246890531964E-16,4.12654611421307E-33));
#7739=DIRECTION('',(0.,0.,-1.));
#7740=DIRECTION('',(-1.,1.60246890531964E-16,0.));
#7741=DIRECTION('center_axis',(0.866025403784439,-0.5,0.));
#7742=DIRECTION('ref_axis',(-0.5,-0.866025403784439,0.));
#7743=DIRECTION('',(-0.5,-0.866025403784439,-9.86805318295748E-20));
#7744=DIRECTION('',(-0.5,-0.866025403784439,0.));
#7745=DIRECTION('center_axis',(0.,0.,-1.));
#7746=DIRECTION('ref_axis',(-1.,0.,0.));
#7747=DIRECTION('center_axis',(0.,0.,1.));
#7748=DIRECTION('ref_axis',(1.,0.,0.));
#7749=DIRECTION('center_axis',(0.,0.,-1.));
#7750=DIRECTION('ref_axis',(1.,0.,0.));
#7751=DIRECTION('center_axis',(-4.10828654779316E-33,1.13946463231163E-19,
-1.));
#7752=DIRECTION('ref_axis',(1.,0.,0.));
#7753=DIRECTION('',(0.,0.,-1.));
#7754=DIRECTION('center_axis',(0.,0.,-1.));
#7755=DIRECTION('ref_axis',(1.,0.,0.));
#7756=DIRECTION('center_axis',(-4.10828654779316E-33,1.13946463231163E-19,
-1.));
#7757=DIRECTION('ref_axis',(1.,0.,0.));
#7758=DIRECTION('',(0.,0.,-1.));
#7759=DIRECTION('center_axis',(4.10828654779316E-33,-1.13946463231163E-19,
1.));
#7760=DIRECTION('ref_axis',(1.,0.,0.));
#7761=DIRECTION('center_axis',(0.,0.,-1.));
#7762=DIRECTION('ref_axis',(1.,0.,0.));
#7763=DIRECTION('center_axis',(-4.10828654779316E-33,1.13946463231163E-19,
-1.));
#7764=DIRECTION('ref_axis',(1.,0.,0.));
#7765=DIRECTION('',(0.,0.,-1.));
#7766=DIRECTION('center_axis',(4.10828654779316E-33,-1.13946463231163E-19,
1.));
#7767=DIRECTION('ref_axis',(1.,0.,0.));
#7768=DIRECTION('center_axis',(0.,0.,-1.));
#7769=DIRECTION('ref_axis',(1.,0.,0.));
#7770=DIRECTION('center_axis',(-4.10828654779316E-33,1.13946463231163E-19,
-1.));
#7771=DIRECTION('ref_axis',(1.,0.,0.));
#7772=DIRECTION('',(0.,0.,-1.));
#7773=DIRECTION('center_axis',(0.,0.,-1.));
#7774=DIRECTION('ref_axis',(1.,0.,0.));
#7775=DIRECTION('',(0.,0.,-1.));
#7776=DIRECTION('center_axis',(0.,0.,1.));
#7777=DIRECTION('ref_axis',(1.,0.,0.));
#7778=DIRECTION('center_axis',(0.,0.,-1.));
#7779=DIRECTION('ref_axis',(1.,0.,0.));
#7780=DIRECTION('',(0.,0.,-1.));
#7781=DIRECTION('center_axis',(0.,0.,1.));
#7782=DIRECTION('ref_axis',(1.,0.,0.));
#7783=DIRECTION('center_axis',(0.,-1.,0.));
#7784=DIRECTION('ref_axis',(-1.,0.,0.));
#7785=DIRECTION('',(0.0523359562429438,0.,0.998629534754574));
#7786=DIRECTION('',(1.,0.,0.));
#7787=DIRECTION('',(-0.0523359562429438,0.,-0.998629534754574));
#7788=DIRECTION('',(1.,0.,0.));
#7789=DIRECTION('center_axis',(0.,-1.,0.));
#7790=DIRECTION('ref_axis',(-1.,0.,0.));
#7791=DIRECTION('',(0.,0.,-1.));
#7792=DIRECTION('',(1.,0.,0.));
#7793=DIRECTION('',(0.,0.,1.));
#7794=DIRECTION('',(1.,0.,0.));
#7795=DIRECTION('center_axis',(0.,-1.,0.));
#7796=DIRECTION('ref_axis',(-1.,0.,0.));
#7797=DIRECTION('',(0.,0.,-1.));
#7798=DIRECTION('',(1.,0.,0.));
#7799=DIRECTION('',(0.,0.,1.));
#7800=DIRECTION('',(1.,0.,0.));
#7801=DIRECTION('center_axis',(0.,-1.,0.));
#7802=DIRECTION('ref_axis',(-1.,0.,0.));
#7803=DIRECTION('',(0.,0.,-1.));
#7804=DIRECTION('',(1.,0.,0.));
#7805=DIRECTION('',(0.,0.,1.));
#7806=DIRECTION('',(1.,0.,0.));
#7807=DIRECTION('center_axis',(0.,1.,0.));
#7808=DIRECTION('ref_axis',(1.,0.,0.));
#7809=DIRECTION('',(-0.0523359562429438,0.,-0.998629534754574));
#7810=DIRECTION('',(-1.,0.,0.));
#7811=DIRECTION('',(0.0523359562429438,0.,0.998629534754574));
#7812=DIRECTION('',(-1.,0.,0.));
#7813=DIRECTION('center_axis',(0.,1.,0.));
#7814=DIRECTION('ref_axis',(1.,0.,0.));
#7815=DIRECTION('',(0.,0.,1.));
#7816=DIRECTION('',(-1.,0.,0.));
#7817=DIRECTION('',(0.,0.,-1.));
#7818=DIRECTION('',(-1.,0.,0.));
#7819=DIRECTION('center_axis',(0.,1.,0.));
#7820=DIRECTION('ref_axis',(1.,0.,0.));
#7821=DIRECTION('',(0.,0.,1.));
#7822=DIRECTION('',(-1.,0.,0.));
#7823=DIRECTION('',(0.,0.,-1.));
#7824=DIRECTION('',(-1.,0.,0.));
#7825=DIRECTION('center_axis',(0.,0.,1.));
#7826=DIRECTION('ref_axis',(1.,0.,0.));
#7827=DIRECTION('center_axis',(0.,0.,1.));
#7828=DIRECTION('ref_axis',(1.,0.,0.));
#7829=DIRECTION('center_axis',(0.,0.,1.));
#7830=DIRECTION('ref_axis',(1.,0.,0.));
#7831=DIRECTION('center_axis',(0.,0.,1.));
#7832=DIRECTION('ref_axis',(1.,0.,0.));
#7833=DIRECTION('center_axis',(0.,0.,1.));
#7834=DIRECTION('ref_axis',(1.,0.,0.));
#7835=DIRECTION('',(0.,1.,0.));
#7836=DIRECTION('',(0.,-1.,0.));
#7837=DIRECTION('center_axis',(0.,0.,1.));
#7838=DIRECTION('ref_axis',(1.,0.,0.));
#7839=DIRECTION('',(0.,-1.,0.));
#7840=DIRECTION('',(0.,1.,0.));
#7841=DIRECTION('center_axis',(0.,0.,1.));
#7842=DIRECTION('ref_axis',(1.,0.,0.));
#7843=DIRECTION('',(0.,-1.,0.));
#7844=DIRECTION('',(0.,1.,0.));
#7845=DIRECTION('center_axis',(0.,0.,1.));
#7846=DIRECTION('ref_axis',(1.,0.,0.));
#7847=DIRECTION('',(0.,-1.,0.));
#7848=DIRECTION('',(-1.,0.,0.));
#7849=DIRECTION('',(0.,1.,0.));
#7850=DIRECTION('center_axis',(0.,1.,0.));
#7851=DIRECTION('ref_axis',(1.,0.,0.));
#7852=DIRECTION('',(0.,0.,1.));
#7853=DIRECTION('',(-1.,0.,0.));
#7854=DIRECTION('',(0.,0.,-1.));
#7855=DIRECTION('center_axis',(-1.,0.,0.));
#7856=DIRECTION('ref_axis',(0.,-1.,0.));
#7857=DIRECTION('',(0.,-1.,0.));
#7858=DIRECTION('center_axis',(1.,0.,0.));
#7859=DIRECTION('ref_axis',(0.,1.,0.));
#7860=DIRECTION('',(0.,1.,0.));
#7861=DIRECTION('',(0.,1.,0.));
#7862=DIRECTION('center_axis',(1.,0.,0.));
#7863=DIRECTION('ref_axis',(0.,1.,0.));
#7864=DIRECTION('',(0.,1.,0.));
#7865=DIRECTION('',(0.,1.,1.13946463231163E-19));
#7866=DIRECTION('',(0.,1.,0.));
#7867=DIRECTION('center_axis',(1.,0.,0.));
#7868=DIRECTION('ref_axis',(0.,1.,0.));
#7869=DIRECTION('',(0.,1.,0.));
#7870=DIRECTION('',(0.,1.,1.13946463231163E-19));
#7871=DIRECTION('',(0.,1.,0.));
#7872=DIRECTION('center_axis',(0.998629534754574,0.,-0.0523359562429438));
#7873=DIRECTION('ref_axis',(-0.0523359562429438,0.,-0.998629534754574));
#7874=DIRECTION('',(0.,-1.,0.));
#7875=DIRECTION('',(-5.97168109510197E-21,-1.,-1.13946463231163E-19));
#7876=DIRECTION('',(0.,-1.,0.));
#7877=DIRECTION('center_axis',(0.,0.,1.));
#7878=DIRECTION('ref_axis',(1.,0.,0.));
#7879=DIRECTION('',(0.,-1.,0.));
#7880=DIRECTION('',(0.,-1.,0.));
#7881=DIRECTION('',(0.,-1.,0.));
#7882=DIRECTION('',(0.,1.,0.));
#7883=DIRECTION('',(0.,-1.,0.));
#7884=DIRECTION('',(0.,1.,0.));
#7885=DIRECTION('',(0.,-1.,0.));
#7886=DIRECTION('',(0.,-1.,0.));
#7887=DIRECTION('',(0.,-1.,0.));
#7888=DIRECTION('',(0.,1.,0.));
#7889=DIRECTION('',(0.,1.,0.));
#7890=DIRECTION('center_axis',(0.,0.,1.));
#7891=DIRECTION('ref_axis',(1.,0.,0.));
#7892=DIRECTION('',(0.,0.,-1.));
#7893=DIRECTION('center_axis',(0.,0.,1.));
#7894=DIRECTION('ref_axis',(1.,0.,0.));
#7895=DIRECTION('center_axis',(4.10828654779316E-33,-1.13946463231163E-19,
1.));
#7896=DIRECTION('ref_axis',(1.,0.,0.));
#7897=DIRECTION('',(0.,0.,-1.));
#7898=DIRECTION('center_axis',(1.,0.,0.));
#7899=DIRECTION('ref_axis',(0.,1.,0.));
#7900=DIRECTION('',(0.,1.,1.13946463231163E-19));
#7901=DIRECTION('center_axis',(0.99852593895705,0.0542765992849681,9.38276897523041E-9));
#7902=DIRECTION('ref_axis',(0.0541946171271057,-0.99701772369063,0.0549418066794405));
#7903=DIRECTION('center_axis',(4.10828654779316E-33,-1.13946463231163E-19,
1.));
#7904=DIRECTION('ref_axis',(1.,0.,-4.10828654779316E-33));
#7905=DIRECTION('',(5.97168109510217E-21,-1.,-1.13946463231163E-19));
#7906=DIRECTION('center_axis',(-1.,0.,0.));
#7907=DIRECTION('ref_axis',(0.,-1.,0.));
#7908=DIRECTION('',(0.,-1.,-1.13946463231163E-19));
#7909=DIRECTION('center_axis',(4.10828654779316E-33,-1.13946463231163E-19,
1.));
#7910=DIRECTION('ref_axis',(1.,0.,-4.10828654779316E-33));
#7911=DIRECTION('center_axis',(-1.,0.,0.));
#7912=DIRECTION('ref_axis',(0.,-1.,0.));
#7913=DIRECTION('',(0.,-1.,-1.13946463231163E-19));
#7914=DIRECTION('center_axis',(4.10828654779316E-33,-1.13946463231163E-19,
1.));
#7915=DIRECTION('ref_axis',(1.,0.,-4.10828654779316E-33));
#7916=DIRECTION('center_axis',(-1.,0.,0.));
#7917=DIRECTION('ref_axis',(0.,-1.,0.));
#7918=DIRECTION('',(0.,-1.,-1.13946463231163E-19));
#7919=DIRECTION('center_axis',(-0.996961060527779,0.0779015005717205,0.));
#7920=DIRECTION('ref_axis',(0.,0.,1.));
#7921=DIRECTION('center_axis',(4.10828654779316E-33,-1.13946463231163E-19,
1.));
#7922=DIRECTION('ref_axis',(1.,0.,-4.10828654779316E-33));
#7923=DIRECTION('',(5.97168109510197E-21,1.,1.13946463231163E-19));
#7924=DIRECTION('center_axis',(-0.996961060527779,-0.0779015005717276,-4.485055189269E-15));
#7925=DIRECTION('ref_axis',(-0.0777791112471086,0.995394757055134,0.0560329142626144));
#7926=DIRECTION('center_axis',(-0.377317868652411,-0.840644185582845,0.388521015186253));
#7927=DIRECTION('ref_axis',(-0.58566693710526,0.541587807512093,0.603056287203763));
#7928=DIRECTION('center_axis',(7.41164423166535E-16,1.,0.));
#7929=DIRECTION('ref_axis',(0.,0.,1.));
#7930=DIRECTION('center_axis',(0.0522650005536027,-0.0520548592672972,0.997275619547472));
#7931=DIRECTION('ref_axis',(-0.998629534754574,7.40148683083438E-16,0.0523359562429445));
#7932=DIRECTION('center_axis',(0.376559988603802,-0.837471124372148,0.396036224133039));
#7933=DIRECTION('ref_axis',(0.577069986161316,0.546481578685729,0.606916893181374));
#7934=DIRECTION('center_axis',(0.998525938475037,-0.0542766081525538,0.));
#7935=DIRECTION('ref_axis',(0.,0.,1.));
#7936=DIRECTION('center_axis',(-0.0522648366634829,-0.0521149007022807,
0.997272492337641));
#7937=DIRECTION('ref_axis',(0.0541946171271058,0.99701772369063,0.0549418066794413));
#7938=DIRECTION('center_axis',(5.32220538281047E-11,1.,-1.01553728389566E-9));
#7939=DIRECTION('ref_axis',(0.998629534754574,0.,0.0523359562429456));
#7940=DIRECTION('center_axis',(0.37731786865241,-0.840644185582843,-0.388521015186259));
#7941=DIRECTION('ref_axis',(-0.585666937105255,-0.541587807512096,0.603056287203765));
#7942=DIRECTION('center_axis',(0.0522650005536027,0.0520548592672965,0.997275619547472));
#7943=DIRECTION('ref_axis',(-0.0777791112471059,-0.995394757055134,0.0560329142626137));
#7944=DIRECTION('center_axis',(0.,-1.,0.));
#7945=DIRECTION('ref_axis',(-0.998629534754574,0.,0.0523359562429439));
#7946=DIRECTION('center_axis',(5.97168109510197E-21,1.,1.13946463231163E-19));
#7947=DIRECTION('ref_axis',(-0.688354575693753,0.,0.725374371012288));
#7948=DIRECTION('center_axis',(-0.376559987018669,-0.837471124206646,-0.396036225990193));
#7949=DIRECTION('ref_axis',(0.577069983350267,-0.54648157893936,0.606916895625808));
#7950=DIRECTION('center_axis',(-0.0522648366634817,0.0521149007022785,0.997272492337641));
#7951=DIRECTION('ref_axis',(0.998629534754574,0.,0.052335956242946));
#7952=DIRECTION('center_axis',(1.01693095242295E-9,-1.,0.));
#7953=DIRECTION('ref_axis',(0.,0.,1.));
#7954=DIRECTION('center_axis',(5.97168109510217E-21,-1.,-1.13946463231163E-19));
#7955=DIRECTION('ref_axis',(0.688354575693753,0.,0.725374371012289));
#7956=DIRECTION('',(-5.97168109510217E-21,1.,1.13946463231163E-19));
#7957=DIRECTION('center_axis',(-0.998629534754574,0.,-0.0523359562429455));
#7958=DIRECTION('ref_axis',(-0.0523359562429455,0.,0.998629534754574));
#7959=DIRECTION('center_axis',(-0.377317868652411,-0.840644185582845,0.388521015186254));
#7960=DIRECTION('ref_axis',(-0.585666937105261,0.541587807512092,0.603056287203763));
#7961=DIRECTION('center_axis',(7.41164423166535E-16,1.,0.));
#7962=DIRECTION('ref_axis',(0.,0.,1.));
#7963=DIRECTION('center_axis',(-0.996961060527779,-0.0779015005717276,-4.485055189269E-15));
#7964=DIRECTION('ref_axis',(-0.0777791112471086,0.995394757055134,0.0560329142626144));
#7965=DIRECTION('center_axis',(0.0522650005536027,-0.0520548592672972,0.997275619547472));
#7966=DIRECTION('ref_axis',(-0.998629534754574,7.40148683083438E-16,0.0523359562429445));
#7967=DIRECTION('center_axis',(0.376559988603802,-0.837471124372148,0.396036224133039));
#7968=DIRECTION('ref_axis',(0.577069986161311,0.546481578685732,0.606916893181376));
#7969=DIRECTION('center_axis',(0.998525938475037,-0.0542766081525538,0.));
#7970=DIRECTION('ref_axis',(0.,0.,1.));
#7971=DIRECTION('center_axis',(5.32220538281047E-11,1.,-1.01553728389566E-9));
#7972=DIRECTION('ref_axis',(0.998629534754574,0.,0.0523359562429456));
#7973=DIRECTION('center_axis',(-0.0522648366634829,-0.0521149007022807,
0.997272492337641));
#7974=DIRECTION('ref_axis',(0.0541946171271058,0.99701772369063,0.0549418066794413));
#7975=DIRECTION('center_axis',(0.37731786865241,-0.840644185582843,-0.388521015186259));
#7976=DIRECTION('ref_axis',(-0.585666937105255,-0.541587807512095,0.603056287203766));
#7977=DIRECTION('center_axis',(-0.996961060527779,0.0779015005717205,0.));
#7978=DIRECTION('ref_axis',(0.,0.,1.));
#7979=DIRECTION('center_axis',(0.,-1.,0.));
#7980=DIRECTION('ref_axis',(-0.998629534754574,0.,0.0523359562429439));
#7981=DIRECTION('center_axis',(0.0522650005536027,0.0520548592672965,0.997275619547472));
#7982=DIRECTION('ref_axis',(-0.0777791112471059,-0.995394757055134,0.0560329142626137));
#7983=DIRECTION('center_axis',(5.97168109510197E-21,1.,1.13946463231163E-19));
#7984=DIRECTION('ref_axis',(-0.688354575693753,0.,0.725374371012289));
#7985=DIRECTION('',(-5.97168109510197E-21,-1.,-1.13946463231163E-19));
#7986=DIRECTION('',(5.97168109510197E-21,1.,1.13946463231163E-19));
#7987=DIRECTION('center_axis',(-0.376559987018669,-0.837471124206646,-0.396036225990194));
#7988=DIRECTION('ref_axis',(0.577069983350267,-0.546481578939359,0.606916895625808));
#7989=DIRECTION('center_axis',(-0.0522648366634817,0.0521149007022785,0.997272492337641));
#7990=DIRECTION('ref_axis',(0.998629534754574,0.,0.052335956242946));
#7991=DIRECTION('center_axis',(1.01693095242295E-9,-1.,0.));
#7992=DIRECTION('ref_axis',(0.,0.,1.));
#7993=DIRECTION('center_axis',(0.99852593895705,0.0542765992849681,9.38276897523041E-9));
#7994=DIRECTION('ref_axis',(0.0541946171271057,-0.99701772369063,0.0549418066794405));
#7995=DIRECTION('center_axis',(5.97168109510217E-21,-1.,-1.13946463231163E-19));
#7996=DIRECTION('ref_axis',(0.688354575693753,0.,0.725374371012289));
#7997=DIRECTION('',(-5.97168109510217E-21,1.,1.13946463231163E-19));
#7998=DIRECTION('',(5.97168109510217E-21,-1.,-1.13946463231163E-19));
#7999=DIRECTION('center_axis',(0.998629534754574,0.,-0.0523359562429438));
#8000=DIRECTION('ref_axis',(-0.0523359562429438,0.,-0.998629534754574));
#8001=DIRECTION('center_axis',(4.10828654779316E-33,-1.13946463231163E-19,
1.));
#8002=DIRECTION('ref_axis',(1.,0.,-4.10828654779316E-33));
#8003=DIRECTION('center_axis',(-0.998629534754574,0.,-0.0523359562429455));
#8004=DIRECTION('ref_axis',(-0.0523359562429455,0.,0.998629534754574));
#8005=DIRECTION('axis',(0.,0.,1.));
#8006=DIRECTION('refdir',(1.,0.,0.));
#8007=DIRECTION('center_axis',(0.,0.,1.));
#8008=DIRECTION('ref_axis',(1.,0.,0.));
#8009=DIRECTION('',(0.,0.,-1.));
#8010=DIRECTION('center_axis',(0.,0.,-1.));
#8011=DIRECTION('ref_axis',(1.,0.,0.));
#8012=DIRECTION('center_axis',(0.,0.,1.));
#8013=DIRECTION('ref_axis',(1.,0.,0.));
#8014=DIRECTION('',(0.,0.,-1.));
#8015=DIRECTION('center_axis',(0.,0.,1.));
#8016=DIRECTION('ref_axis',(1.,0.,0.));
#8017=DIRECTION('',(0.,0.,-1.));
#8018=DIRECTION('center_axis',(0.,0.,1.));
#8019=DIRECTION('ref_axis',(1.,0.,0.));
#8020=DIRECTION('',(0.,0.,-1.));
#8021=DIRECTION('center_axis',(0.,0.,1.));
#8022=DIRECTION('ref_axis',(1.,0.,0.));
#8023=DIRECTION('',(0.,0.,-1.));
#8024=DIRECTION('center_axis',(0.,0.,1.));
#8025=DIRECTION('ref_axis',(1.,0.,0.));
#8026=DIRECTION('',(0.,0.,-1.));
#8027=DIRECTION('center_axis',(0.,0.,1.));
#8028=DIRECTION('ref_axis',(1.,0.,0.));
#8029=DIRECTION('',(0.,0.,-1.));
#8030=DIRECTION('center_axis',(0.,0.,1.));
#8031=DIRECTION('ref_axis',(1.,0.,0.));
#8032=DIRECTION('',(0.,0.,-1.));
#8033=DIRECTION('center_axis',(0.,0.,1.));
#8034=DIRECTION('ref_axis',(1.,0.,0.));
#8035=DIRECTION('',(0.,0.,-1.));
#8036=DIRECTION('center_axis',(0.,0.,1.));
#8037=DIRECTION('ref_axis',(1.,0.,0.));
#8038=DIRECTION('',(0.,0.,-1.));
#8039=DIRECTION('center_axis',(0.,0.,1.));
#8040=DIRECTION('ref_axis',(1.,0.,0.));
#8041=DIRECTION('',(0.,0.,-1.));
#8042=DIRECTION('center_axis',(0.,0.,1.));
#8043=DIRECTION('ref_axis',(1.,0.,0.));
#8044=DIRECTION('',(0.,0.,-1.));
#8045=DIRECTION('center_axis',(0.,0.,1.));
#8046=DIRECTION('ref_axis',(1.,0.,0.));
#8047=DIRECTION('',(0.,0.,-1.));
#8048=DIRECTION('center_axis',(0.,0.,1.));
#8049=DIRECTION('ref_axis',(1.,0.,0.));
#8050=DIRECTION('',(0.,0.,-1.));
#8051=DIRECTION('center_axis',(0.,0.,1.));
#8052=DIRECTION('ref_axis',(1.,0.,0.));
#8053=DIRECTION('',(0.,0.,-1.));
#8054=DIRECTION('center_axis',(0.,0.,1.));
#8055=DIRECTION('ref_axis',(1.,0.,0.));
#8056=DIRECTION('',(0.,0.,-1.));
#8057=DIRECTION('center_axis',(0.,0.,1.));
#8058=DIRECTION('ref_axis',(1.,0.,0.));
#8059=DIRECTION('',(0.,0.,-1.));
#8060=DIRECTION('center_axis',(0.,0.,1.));
#8061=DIRECTION('ref_axis',(1.,0.,0.));
#8062=DIRECTION('',(0.,0.,-1.));
#8063=DIRECTION('center_axis',(0.,0.,1.));
#8064=DIRECTION('ref_axis',(1.,0.,0.));
#8065=DIRECTION('',(0.,0.,-1.));
#8066=DIRECTION('center_axis',(0.,0.,1.));
#8067=DIRECTION('ref_axis',(1.,0.,0.));
#8068=DIRECTION('',(0.,0.,-1.));
#8069=DIRECTION('center_axis',(0.,0.,1.));
#8070=DIRECTION('ref_axis',(1.,0.,0.));
#8071=DIRECTION('',(0.,0.,-1.));
#8072=DIRECTION('center_axis',(0.,0.,1.));
#8073=DIRECTION('ref_axis',(1.,0.,0.));
#8074=DIRECTION('',(0.,0.,-1.));
#8075=DIRECTION('center_axis',(0.,0.,1.));
#8076=DIRECTION('ref_axis',(1.,0.,0.));
#8077=DIRECTION('',(0.,0.,-1.));
#8078=DIRECTION('center_axis',(0.,0.,1.));
#8079=DIRECTION('ref_axis',(1.,0.,0.));
#8080=DIRECTION('',(0.,0.,-1.));
#8081=DIRECTION('center_axis',(0.,0.,1.));
#8082=DIRECTION('ref_axis',(1.,0.,0.));
#8083=DIRECTION('',(0.,0.,-1.));
#8084=DIRECTION('center_axis',(0.,0.,1.));
#8085=DIRECTION('ref_axis',(1.,0.,0.));
#8086=DIRECTION('',(0.,0.,-1.));
#8087=DIRECTION('center_axis',(0.,0.,1.));
#8088=DIRECTION('ref_axis',(1.,0.,0.));
#8089=DIRECTION('',(0.,0.,-1.));
#8090=DIRECTION('center_axis',(0.,0.,1.));
#8091=DIRECTION('ref_axis',(1.,0.,0.));
#8092=DIRECTION('',(0.,0.,-1.));
#8093=DIRECTION('center_axis',(0.,0.,1.));
#8094=DIRECTION('ref_axis',(1.,0.,0.));
#8095=DIRECTION('',(0.,0.,-1.));
#8096=DIRECTION('center_axis',(0.,0.,1.));
#8097=DIRECTION('ref_axis',(1.,0.,0.));
#8098=DIRECTION('',(0.,0.,-1.));
#8099=DIRECTION('center_axis',(0.,0.,1.));
#8100=DIRECTION('ref_axis',(1.,-2.42503376499884E-13,0.));
#8101=DIRECTION('',(0.,0.,1.));
#8102=DIRECTION('center_axis',(0.,0.,-1.));
#8103=DIRECTION('ref_axis',(1.,-2.42503376499884E-13,0.));
#8104=DIRECTION('center_axis',(0.,0.,1.));
#8105=DIRECTION('ref_axis',(1.,-2.42503376499884E-13,0.));
#8106=DIRECTION('',(0.,0.,1.));
#8107=DIRECTION('center_axis',(0.,0.,1.));
#8108=DIRECTION('ref_axis',(1.,-2.42503376499884E-13,0.));
#8109=DIRECTION('',(0.,0.,1.));
#8110=DIRECTION('center_axis',(0.,0.,1.));
#8111=DIRECTION('ref_axis',(1.,-2.42503376499884E-13,0.));
#8112=DIRECTION('',(0.,0.,1.));
#8113=DIRECTION('center_axis',(0.,0.,1.));
#8114=DIRECTION('ref_axis',(1.,-2.42503376499884E-13,0.));
#8115=DIRECTION('',(0.,0.,1.));
#8116=DIRECTION('center_axis',(0.,0.,1.));
#8117=DIRECTION('ref_axis',(1.,-2.42503376499884E-13,0.));
#8118=DIRECTION('',(0.,0.,1.));
#8119=DIRECTION('center_axis',(0.,0.,1.));
#8120=DIRECTION('ref_axis',(1.,-2.42503376499884E-13,0.));
#8121=DIRECTION('',(0.,0.,1.));
#8122=DIRECTION('center_axis',(0.,0.,1.));
#8123=DIRECTION('ref_axis',(1.,-2.42503376499884E-13,0.));
#8124=DIRECTION('',(0.,0.,1.));
#8125=DIRECTION('center_axis',(0.,0.,1.));
#8126=DIRECTION('ref_axis',(1.,-2.42503376499884E-13,0.));
#8127=DIRECTION('',(0.,0.,1.));
#8128=DIRECTION('center_axis',(0.,0.,1.));
#8129=DIRECTION('ref_axis',(1.,-2.42503376499884E-13,0.));
#8130=DIRECTION('',(0.,0.,1.));
#8131=DIRECTION('center_axis',(0.,0.,1.));
#8132=DIRECTION('ref_axis',(1.,-2.42503376499884E-13,0.));
#8133=DIRECTION('',(0.,0.,1.));
#8134=DIRECTION('center_axis',(0.,0.,1.));
#8135=DIRECTION('ref_axis',(1.,-2.42503376499884E-13,0.));
#8136=DIRECTION('',(0.,0.,1.));
#8137=DIRECTION('center_axis',(0.,0.,1.));
#8138=DIRECTION('ref_axis',(1.,-2.42503376499884E-13,0.));
#8139=DIRECTION('',(0.,0.,1.));
#8140=DIRECTION('center_axis',(0.,0.,1.));
#8141=DIRECTION('ref_axis',(1.,-2.42503376499884E-13,0.));
#8142=DIRECTION('',(0.,0.,1.));
#8143=DIRECTION('center_axis',(0.,0.,1.));
#8144=DIRECTION('ref_axis',(1.,-2.42503376499884E-13,0.));
#8145=DIRECTION('',(0.,0.,1.));
#8146=DIRECTION('center_axis',(0.,0.,1.));
#8147=DIRECTION('ref_axis',(1.,-2.42503376499884E-13,0.));
#8148=DIRECTION('',(0.,0.,1.));
#8149=DIRECTION('center_axis',(0.,0.,1.));
#8150=DIRECTION('ref_axis',(1.,-2.42503376499884E-13,0.));
#8151=DIRECTION('',(0.,0.,1.));
#8152=DIRECTION('center_axis',(0.,0.,1.));
#8153=DIRECTION('ref_axis',(1.,-2.42503376499884E-13,0.));
#8154=DIRECTION('',(0.,0.,1.));
#8155=DIRECTION('center_axis',(0.,0.,1.));
#8156=DIRECTION('ref_axis',(1.,-2.42503376499884E-13,0.));
#8157=DIRECTION('',(0.,0.,1.));
#8158=DIRECTION('center_axis',(0.,0.,1.));
#8159=DIRECTION('ref_axis',(1.,-2.42503376499884E-13,0.));
#8160=DIRECTION('',(0.,0.,1.));
#8161=DIRECTION('center_axis',(0.,0.,1.));
#8162=DIRECTION('ref_axis',(1.,-2.42503376499884E-13,0.));
#8163=DIRECTION('',(0.,0.,1.));
#8164=DIRECTION('center_axis',(0.,0.,1.));
#8165=DIRECTION('ref_axis',(1.,-2.42503376499884E-13,0.));
#8166=DIRECTION('',(0.,0.,1.));
#8167=DIRECTION('center_axis',(0.,0.,1.));
#8168=DIRECTION('ref_axis',(1.,-2.42503376499884E-13,0.));
#8169=DIRECTION('',(0.,0.,1.));
#8170=DIRECTION('center_axis',(0.,0.,1.));
#8171=DIRECTION('ref_axis',(1.,-2.42503376499884E-13,0.));
#8172=DIRECTION('',(0.,0.,1.));
#8173=DIRECTION('center_axis',(0.,0.,1.));
#8174=DIRECTION('ref_axis',(1.,-2.42503376499884E-13,0.));
#8175=DIRECTION('',(0.,0.,1.));
#8176=DIRECTION('center_axis',(0.,0.,1.));
#8177=DIRECTION('ref_axis',(1.,-2.42503376499884E-13,0.));
#8178=DIRECTION('',(0.,0.,1.));
#8179=DIRECTION('center_axis',(0.,0.,1.));
#8180=DIRECTION('ref_axis',(1.,-2.42503376499884E-13,0.));
#8181=DIRECTION('',(0.,0.,1.));
#8182=DIRECTION('center_axis',(0.,0.,1.));
#8183=DIRECTION('ref_axis',(1.,-2.42503376499884E-13,0.));
#8184=DIRECTION('',(0.,0.,1.));
#8185=DIRECTION('center_axis',(0.,0.,1.));
#8186=DIRECTION('ref_axis',(1.,-2.42503376499884E-13,0.));
#8187=DIRECTION('',(0.,0.,1.));
#8188=DIRECTION('center_axis',(0.,0.,1.));
#8189=DIRECTION('ref_axis',(1.,-2.42503376499884E-13,0.));
#8190=DIRECTION('',(0.,0.,1.));
#8191=DIRECTION('center_axis',(0.,0.,-1.));
#8192=DIRECTION('ref_axis',(1.,0.,0.));
#8193=DIRECTION('center_axis',(0.,0.,-1.));
#8194=DIRECTION('ref_axis',(1.,0.,0.));
#8195=DIRECTION('',(0.707106781186547,8.65956056235493E-17,0.707106781186548));
#8196=DIRECTION('center_axis',(0.,0.,1.));
#8197=DIRECTION('ref_axis',(1.,0.,0.));
#8198=DIRECTION('center_axis',(0.,0.,1.));
#8199=DIRECTION('ref_axis',(1.,-2.42503376499884E-13,0.));
#8200=DIRECTION('center_axis',(0.,0.,-1.));
#8201=DIRECTION('ref_axis',(1.,-2.42503376499884E-13,0.));
#8202=DIRECTION('center_axis',(0.,0.,1.));
#8203=DIRECTION('ref_axis',(1.,0.,0.));
#8204=DIRECTION('center_axis',(-1.92296268638356E-16,-1.,0.));
#8205=DIRECTION('ref_axis',(1.,-1.92296268638356E-16,0.));
#8206=DIRECTION('',(1.,-1.92296268638356E-16,0.));
#8207=DIRECTION('',(0.,0.,1.));
#8208=DIRECTION('',(1.,-1.92296268638356E-16,0.));
#8209=DIRECTION('',(0.,0.,1.));
#8210=DIRECTION('center_axis',(-0.866025403784439,-0.5,0.));
#8211=DIRECTION('ref_axis',(0.5,-0.866025403784439,0.));
#8212=DIRECTION('',(0.5,-0.866025403784439,0.));
#8213=DIRECTION('',(0.,0.,1.));
#8214=DIRECTION('',(0.5,-0.866025403784439,0.));
#8215=DIRECTION('center_axis',(-0.866025403784439,0.5,0.));
#8216=DIRECTION('ref_axis',(-0.5,-0.866025403784439,0.));
#8217=DIRECTION('',(-0.5,-0.866025403784439,0.));
#8218=DIRECTION('',(0.,0.,1.));
#8219=DIRECTION('',(-0.5,-0.866025403784438,0.));
#8220=DIRECTION('center_axis',(1.92296268638356E-16,1.,0.));
#8221=DIRECTION('ref_axis',(-1.,1.92296268638356E-16,0.));
#8222=DIRECTION('',(-1.,1.92296268638356E-16,0.));
#8223=DIRECTION('',(0.,0.,1.));
#8224=DIRECTION('',(-1.,1.92296268638356E-16,0.));
#8225=DIRECTION('center_axis',(0.866025403784439,0.5,0.));
#8226=DIRECTION('ref_axis',(-0.5,0.866025403784439,0.));
#8227=DIRECTION('',(-0.5,0.866025403784439,0.));
#8228=DIRECTION('',(0.,0.,1.));
#8229=DIRECTION('',(-0.5,0.866025403784439,0.));
#8230=DIRECTION('center_axis',(0.866025403784439,-0.5,0.));
#8231=DIRECTION('ref_axis',(0.5,0.866025403784439,0.));
#8232=DIRECTION('',(0.5,0.866025403784439,0.));
#8233=DIRECTION('',(0.5,0.866025403784439,0.));
#8234=DIRECTION('center_axis',(0.,0.,1.));
#8235=DIRECTION('ref_axis',(1.,0.,0.));
#8236=DIRECTION('center_axis',(0.,0.,1.));
#8237=DIRECTION('ref_axis',(1.,0.,0.));
#8238=DIRECTION('center_axis',(0.,0.,1.));
#8239=DIRECTION('ref_axis',(1.,0.,0.));
#8240=DIRECTION('center_axis',(0.,0.,1.));
#8241=DIRECTION('ref_axis',(1.,0.,0.));
#8242=DIRECTION('',(0.,0.,-1.));
#8243=DIRECTION('center_axis',(0.,0.,1.));
#8244=DIRECTION('ref_axis',(1.,0.,0.));
#8245=DIRECTION('center_axis',(0.,0.,1.));
#8246=DIRECTION('ref_axis',(1.,0.,0.));
#8247=DIRECTION('center_axis',(0.,0.,1.));
#8248=DIRECTION('ref_axis',(1.,0.,0.));
#8249=DIRECTION('axis',(0.,0.,1.));
#8250=DIRECTION('refdir',(1.,0.,0.));
#8251=DIRECTION('center_axis',(0.,0.,-1.));
#8252=DIRECTION('ref_axis',(1.,0.,0.));
#8253=DIRECTION('',(0.,0.,-1.));
#8254=DIRECTION('center_axis',(0.,0.,-1.));
#8255=DIRECTION('ref_axis',(1.,0.,0.));
#8256=DIRECTION('center_axis',(0.,0.,-1.));
#8257=DIRECTION('ref_axis',(1.,0.,0.));
#8258=DIRECTION('',(0.,0.,-1.));
#8259=DIRECTION('center_axis',(0.,0.,-1.));
#8260=DIRECTION('ref_axis',(1.,0.,0.));
#8261=DIRECTION('center_axis',(0.,0.,-1.));
#8262=DIRECTION('ref_axis',(1.,0.,0.));
#8263=DIRECTION('',(0.,0.,-1.));
#8264=DIRECTION('center_axis',(0.,0.,-1.));
#8265=DIRECTION('ref_axis',(1.,0.,0.));
#8266=DIRECTION('',(0.,0.,-1.));
#8267=DIRECTION('center_axis',(0.,0.,-1.));
#8268=DIRECTION('ref_axis',(0.937385399639056,-0.348293859468591,0.));
#8269=DIRECTION('',(0.,0.,-1.));
#8270=DIRECTION('center_axis',(0.,0.,-1.));
#8271=DIRECTION('ref_axis',(1.,0.,0.));
#8272=DIRECTION('center_axis',(0.,0.,-1.));
#8273=DIRECTION('ref_axis',(0.28361887368566,0.958937085782627,0.));
#8274=DIRECTION('',(1.22464679914735E-16,8.07419868282478E-31,-1.));
#8275=DIRECTION('center_axis',(0.,0.,1.));
#8276=DIRECTION('ref_axis',(1.,6.71554824363804E-15,0.));
#8277=DIRECTION('center_axis',(0.,0.,-1.));
#8278=DIRECTION('ref_axis',(1.,6.71554824363804E-15,0.));
#8279=DIRECTION('',(1.22464679914735E-16,8.07419868282478E-31,-1.));
#8280=DIRECTION('center_axis',(0.,0.,-1.));
#8281=DIRECTION('ref_axis',(1.,6.71554824363804E-15,0.));
#8282=DIRECTION('',(1.22464679914735E-16,8.07419868282478E-31,-1.));
#8283=DIRECTION('center_axis',(0.,0.,-1.));
#8284=DIRECTION('ref_axis',(1.,6.71554824363804E-15,0.));
#8285=DIRECTION('',(1.22464679914735E-16,8.07419868282478E-31,-1.));
#8286=DIRECTION('center_axis',(0.,0.,-1.));
#8287=DIRECTION('ref_axis',(-0.60895050335979,-0.793208222636313,0.));
#8288=DIRECTION('',(1.22464679914735E-16,8.07419868282478E-31,-1.));
#8289=DIRECTION('center_axis',(0.,0.,-1.));
#8290=DIRECTION('ref_axis',(1.,6.71554824363804E-15,0.));
#8291=DIRECTION('center_axis',(0.,0.,-1.));
#8292=DIRECTION('ref_axis',(1.,6.71554824363804E-15,0.));
#8293=DIRECTION('center_axis',(0.,0.,1.));
#8294=DIRECTION('ref_axis',(1.,0.,0.));
#8295=DIRECTION('',(0.5,0.866025403784439,0.));
#8296=DIRECTION('',(-0.5,0.866025403784439,0.));
#8297=DIRECTION('',(-1.,0.,0.));
#8298=DIRECTION('',(-0.5,-0.866025403784439,0.));
#8299=DIRECTION('',(0.5,-0.866025403784439,0.));
#8300=DIRECTION('',(1.,-3.49629579342466E-16,0.));
#8301=DIRECTION('center_axis',(0.,0.,-1.));
#8302=DIRECTION('ref_axis',(1.,0.,0.));
#8303=DIRECTION('center_axis',(-3.49629579342466E-16,-1.,0.));
#8304=DIRECTION('ref_axis',(1.,-3.49629579342466E-16,0.));
#8305=DIRECTION('',(1.,-3.49629579342466E-16,0.));
#8306=DIRECTION('',(0.,0.,1.));
#8307=DIRECTION('',(0.,0.,1.));
#8308=DIRECTION('center_axis',(-0.866025403784439,-0.5,0.));
#8309=DIRECTION('ref_axis',(0.5,-0.866025403784439,0.));
#8310=DIRECTION('',(0.5,-0.866025403784439,0.));
#8311=DIRECTION('',(0.,0.,1.));
#8312=DIRECTION('center_axis',(-0.866025403784439,0.5,0.));
#8313=DIRECTION('ref_axis',(-0.5,-0.866025403784439,0.));
#8314=DIRECTION('',(-0.5,-0.866025403784439,0.));
#8315=DIRECTION('',(0.,0.,1.));
#8316=DIRECTION('center_axis',(0.,1.,0.));
#8317=DIRECTION('ref_axis',(-1.,0.,0.));
#8318=DIRECTION('',(-1.,0.,0.));
#8319=DIRECTION('',(0.,0.,1.));
#8320=DIRECTION('center_axis',(0.866025403784439,0.5,0.));
#8321=DIRECTION('ref_axis',(-0.5,0.866025403784439,0.));
#8322=DIRECTION('',(-0.5,0.866025403784439,0.));
#8323=DIRECTION('',(0.,0.,1.));
#8324=DIRECTION('center_axis',(0.866025403784439,-0.5,0.));
#8325=DIRECTION('ref_axis',(0.5,0.866025403784439,0.));
#8326=DIRECTION('',(0.5,0.866025403784439,0.));
#8327=DIRECTION('center_axis',(0.,0.,1.));
#8328=DIRECTION('ref_axis',(1.,0.,0.));
#8329=DIRECTION('axis',(0.,0.,1.));
#8330=DIRECTION('refdir',(1.,0.,0.));
#8331=DIRECTION('center_axis',(0.,0.,-1.));
#8332=DIRECTION('ref_axis',(1.,0.,0.));
#8333=DIRECTION('center_axis',(1.16928610669829E-31,-5.97538301968883E-32,
-1.));
#8334=DIRECTION('ref_axis',(1.,0.,0.));
#8335=DIRECTION('',(0.,0.,-1.));
#8336=DIRECTION('center_axis',(-6.45616000593692E-32,-1.81182428107391E-19,
1.));
#8337=DIRECTION('ref_axis',(1.,0.,0.));
#8338=DIRECTION('center_axis',(0.,0.,-1.));
#8339=DIRECTION('ref_axis',(1.,0.,0.));
#8340=DIRECTION('center_axis',(1.16928610669829E-31,-5.97538301968883E-32,
-1.));
#8341=DIRECTION('ref_axis',(1.,0.,0.));
#8342=DIRECTION('',(0.,0.,-1.));
#8343=DIRECTION('center_axis',(-6.45616000593692E-32,-1.81182428107391E-19,
1.));
#8344=DIRECTION('ref_axis',(1.,0.,0.));
#8345=DIRECTION('center_axis',(0.,0.,1.));
#8346=DIRECTION('ref_axis',(1.,0.,0.));
#8347=DIRECTION('center_axis',(0.,0.,1.));
#8348=DIRECTION('ref_axis',(1.,0.,0.));
#8349=DIRECTION('center_axis',(0.,0.,-1.));
#8350=DIRECTION('ref_axis',(1.,0.,0.));
#8351=DIRECTION('center_axis',(0.,0.,-1.));
#8352=DIRECTION('ref_axis',(1.,0.,0.));
#8353=DIRECTION('center_axis',(0.,0.,-1.));
#8354=DIRECTION('ref_axis',(1.,0.,0.));
#8355=DIRECTION('',(0.,0.,1.));
#8356=DIRECTION('center_axis',(0.,0.,1.));
#8357=DIRECTION('ref_axis',(1.,0.,0.));
#8358=DIRECTION('center_axis',(0.,0.,1.));
#8359=DIRECTION('ref_axis',(1.,0.,0.));
#8360=DIRECTION('center_axis',(0.,0.,1.));
#8361=DIRECTION('ref_axis',(1.,0.,0.));
#8362=DIRECTION('center_axis',(0.,0.,-1.));
#8363=DIRECTION('ref_axis',(1.,0.,0.));
#8364=DIRECTION('center_axis',(0.,0.,-1.));
#8365=DIRECTION('ref_axis',(1.,0.,0.));
#8366=DIRECTION('center_axis',(0.,0.,-1.));
#8367=DIRECTION('ref_axis',(1.,0.,0.));
#8368=DIRECTION('',(0.,0.,1.));
#8369=DIRECTION('center_axis',(0.,0.,1.));
#8370=DIRECTION('ref_axis',(1.,0.,0.));
#8371=DIRECTION('center_axis',(0.,0.,1.));
#8372=DIRECTION('ref_axis',(1.,0.,0.));
#8373=DIRECTION('center_axis',(0.,0.,1.));
#8374=DIRECTION('ref_axis',(1.,0.,0.));
#8375=DIRECTION('center_axis',(0.,0.,-1.));
#8376=DIRECTION('ref_axis',(1.,0.,0.));
#8377=DIRECTION('center_axis',(0.,0.,-1.));
#8378=DIRECTION('ref_axis',(1.,0.,0.));
#8379=DIRECTION('center_axis',(0.,0.,-1.));
#8380=DIRECTION('ref_axis',(1.,0.,0.));
#8381=DIRECTION('',(0.,0.,1.));
#8382=DIRECTION('center_axis',(0.,0.,1.));
#8383=DIRECTION('ref_axis',(1.,0.,0.));
#8384=DIRECTION('center_axis',(0.,0.,1.));
#8385=DIRECTION('ref_axis',(1.,0.,0.));
#8386=DIRECTION('center_axis',(0.,0.,1.));
#8387=DIRECTION('ref_axis',(1.,0.,0.));
#8388=DIRECTION('center_axis',(0.,0.,-1.));
#8389=DIRECTION('ref_axis',(1.,0.,0.));
#8390=DIRECTION('center_axis',(0.,0.,-1.));
#8391=DIRECTION('ref_axis',(1.,0.,0.));
#8392=DIRECTION('center_axis',(0.,0.,-1.));
#8393=DIRECTION('ref_axis',(1.,0.,0.));
#8394=DIRECTION('',(0.,0.,1.));
#8395=DIRECTION('center_axis',(0.,0.,1.));
#8396=DIRECTION('ref_axis',(1.,0.,0.));
#8397=DIRECTION('center_axis',(0.,0.,-1.));
#8398=DIRECTION('ref_axis',(1.,0.,0.));
#8399=DIRECTION('',(0.,0.,1.));
#8400=DIRECTION('center_axis',(-6.45616000593692E-32,-1.81182428107391E-19,
1.));
#8401=DIRECTION('ref_axis',(1.,0.,0.));
#8402=DIRECTION('center_axis',(0.,0.,-1.));
#8403=DIRECTION('ref_axis',(1.,0.,0.));
#8404=DIRECTION('',(0.,0.,1.));
#8405=DIRECTION('center_axis',(-6.45616000593692E-32,-1.81182428107391E-19,
1.));
#8406=DIRECTION('ref_axis',(1.,0.,0.));
#8407=DIRECTION('center_axis',(0.,0.,-1.));
#8408=DIRECTION('ref_axis',(1.,0.,0.));
#8409=DIRECTION('',(0.,0.,1.));
#8410=DIRECTION('center_axis',(-6.45616000593692E-32,-1.81182428107391E-19,
1.));
#8411=DIRECTION('ref_axis',(1.,0.,0.));
#8412=DIRECTION('center_axis',(0.,0.,-1.));
#8413=DIRECTION('ref_axis',(1.,0.,0.));
#8414=DIRECTION('',(0.,0.,1.));
#8415=DIRECTION('center_axis',(-6.45616000593692E-32,-1.81182428107391E-19,
1.));
#8416=DIRECTION('ref_axis',(1.,0.,0.));
#8417=DIRECTION('center_axis',(0.,1.,0.));
#8418=DIRECTION('ref_axis',(0.,0.,1.));
#8419=DIRECTION('center_axis',(0.998287351281347,-0.0585009766728139,0.));
#8420=DIRECTION('ref_axis',(0.0584117362954384,0.996764512774636,0.0552139034672828));
#8421=DIRECTION('center_axis',(-3.13156554427463E-33,-1.,5.97538301968883E-32));
#8422=DIRECTION('ref_axis',(0.688354575693766,0.,0.725374371012276));
#8423=DIRECTION('center_axis',(1.38968329343724E-15,1.,0.));
#8424=DIRECTION('ref_axis',(0.,0.,1.));
#8425=DIRECTION('',(3.13156554427463E-33,1.,-5.97538301968883E-32));
#8426=DIRECTION('',(-3.13156554427463E-33,-1.,5.97538301968883E-32));
#8427=DIRECTION('center_axis',(0.998287351281345,0.0585009766728351,0.));
#8428=DIRECTION('ref_axis',(0.,0.,1.));
#8429=DIRECTION('center_axis',(0.996325437245183,-0.0856482521607663,0.));
#8430=DIRECTION('ref_axis',(0.,0.,1.));
#8431=DIRECTION('center_axis',(-1.38968329343725E-15,-1.,-6.75000545323542E-30));
#8432=DIRECTION('ref_axis',(-4.85722573273506E-15,0.,1.));
#8433=DIRECTION('center_axis',(-3.13156554427485E-33,1.,-5.97538301968883E-32));
#8434=DIRECTION('ref_axis',(-0.688354575693752,0.,0.72537437101229));
#8435=DIRECTION('center_axis',(1.38968329343726E-15,-1.,0.));
#8436=DIRECTION('ref_axis',(0.,0.,1.));
#8437=DIRECTION('',(3.13156554427485E-33,-1.,5.97538301968883E-32));
#8438=DIRECTION('',(-3.13156554427485E-33,1.,-5.97538301968883E-32));
#8439=DIRECTION('center_axis',(-0.996325437245184,-0.0856482521607654,-4.83937755196581E-15));
#8440=DIRECTION('ref_axis',(-4.85722573273506E-15,0.,1.));
#8441=DIRECTION('center_axis',(0.998629534754574,0.,-0.0523359562429439));
#8442=DIRECTION('ref_axis',(-0.0523359562429439,0.,-0.998629534754574));
#8443=DIRECTION('',(0.,1.,0.));
#8444=DIRECTION('center_axis',(-1.16928610669829E-31,5.97538301968883E-32,
1.));
#8445=DIRECTION('ref_axis',(1.,0.,1.16928610669829E-31));
#8446=DIRECTION('center_axis',(-0.998629534754574,0.,-0.0523359562429402));
#8447=DIRECTION('ref_axis',(-0.0523359562429402,0.,0.998629534754574));
#8448=DIRECTION('',(0.,-1.,0.));
#8449=DIRECTION('center_axis',(-6.45616000593692E-32,-1.81182428107391E-19,
1.));
#8450=DIRECTION('ref_axis',(1.,0.,6.45616000593692E-32));
#8451=DIRECTION('',(0.,0.,1.));
#8452=DIRECTION('',(1.,0.,0.));
#8453=DIRECTION('',(0.,-1.22464679914735E-16,-1.));
#8454=DIRECTION('',(1.,0.,0.));
#8455=DIRECTION('',(0.,-1.22464679914735E-16,-1.));
#8456=DIRECTION('',(1.,0.,0.));
#8457=DIRECTION('',(0.,0.,1.));
#8458=DIRECTION('',(1.,0.,0.));
#8459=DIRECTION('',(0.,0.,1.));
#8460=DIRECTION('',(1.,0.,0.));
#8461=DIRECTION('',(0.,-1.22464679914735E-16,-1.));
#8462=DIRECTION('',(1.,0.,0.));
#8463=DIRECTION('',(0.,0.,1.));
#8464=DIRECTION('',(1.,0.,0.));
#8465=DIRECTION('',(0.,-1.22464679914735E-16,-1.));
#8466=DIRECTION('',(1.,0.,0.));
#8467=DIRECTION('axis',(0.,0.,1.));
#8468=DIRECTION('refdir',(1.,0.,0.));
#8469=DIRECTION('center_axis',(0.,0.,1.));
#8470=DIRECTION('ref_axis',(1.,0.,0.));
#8471=DIRECTION('center_axis',(0.,0.,-1.));
#8472=DIRECTION('ref_axis',(1.,0.,0.));
#8473=DIRECTION('',(0.,0.,-1.));
#8474=DIRECTION('center_axis',(0.,0.,-1.));
#8475=DIRECTION('ref_axis',(1.,0.,0.));
#8476=DIRECTION('center_axis',(0.,0.,1.));
#8477=DIRECTION('ref_axis',(1.,0.,0.));
#8478=DIRECTION('center_axis',(0.,0.,1.));
#8479=DIRECTION('ref_axis',(1.,0.,0.));
#8480=DIRECTION('',(0.,0.,-1.));
#8481=DIRECTION('center_axis',(0.,0.,1.));
#8482=DIRECTION('ref_axis',(1.,0.,0.));
#8483=DIRECTION('center_axis',(0.,0.,1.));
#8484=DIRECTION('ref_axis',(1.,0.,0.));
#8485=DIRECTION('center_axis',(0.,0.,1.));
#8486=DIRECTION('ref_axis',(1.,0.,0.));
#8487=DIRECTION('',(0.,0.,1.));
#8488=DIRECTION('',(1.,0.,0.));
#8489=DIRECTION('',(0.,0.,1.));
#8490=DIRECTION('',(1.,0.,0.));
#8491=DIRECTION('',(0.,-1.22464679914735E-16,-1.));
#8492=DIRECTION('',(1.,0.,0.));
#8493=DIRECTION('',(0.,0.,1.));
#8494=DIRECTION('',(1.,0.,0.));
#8495=DIRECTION('',(0.,0.,1.));
#8496=DIRECTION('',(1.,0.,0.));
#8497=DIRECTION('',(0.,0.,1.));
#8498=DIRECTION('',(1.,0.,0.));
#8499=DIRECTION('',(0.,-1.22464679914735E-16,-1.));
#8500=DIRECTION('',(1.,0.,0.));
#8501=DIRECTION('',(0.,0.,1.));
#8502=DIRECTION('',(1.,0.,0.));
#8503=CARTESIAN_POINT('',(0.,0.,0.));
#8504=CARTESIAN_POINT('',(0.,0.,0.));
#8505=CARTESIAN_POINT('Origin',(6.,-2.5,0.3));
#8506=CARTESIAN_POINT('',(5.83,-2.5,0.6));
#8507=CARTESIAN_POINT('Origin',(6.,-2.5,0.6));
#8508=CARTESIAN_POINT('',(5.83,-2.5,0.));
#8509=CARTESIAN_POINT('',(5.83,-2.5,0.3));
#8510=CARTESIAN_POINT('Origin',(6.,-2.5,0.));
#8511=CARTESIAN_POINT('Origin',(12.8,-2.5,0.3));
#8512=CARTESIAN_POINT('',(12.63,-2.5,0.6));
#8513=CARTESIAN_POINT('Origin',(12.8,-2.5,0.6));
#8514=CARTESIAN_POINT('',(12.63,-2.5,0.));
#8515=CARTESIAN_POINT('',(12.63,-2.5,0.3));
#8516=CARTESIAN_POINT('Origin',(12.8,-2.5,0.));
#8517=CARTESIAN_POINT('Origin',(0.,0.,0.3));
#8518=CARTESIAN_POINT('',(-0.41,5.02105187650415E-17,0.6));
#8519=CARTESIAN_POINT('Origin',(0.,0.,0.6));
#8520=CARTESIAN_POINT('',(-0.41,5.02105187650415E-17,0.));
#8521=CARTESIAN_POINT('',(-0.41,5.02105187650415E-17,0.3));
#8522=CARTESIAN_POINT('Origin',(0.,0.,0.));
#8523=CARTESIAN_POINT('Origin',(-2.2,0.025,0.125));
#8524=CARTESIAN_POINT('',(-2.2,0.2,0.2));
#8525=CARTESIAN_POINT('',(-2.2,-0.0999999999999999,0.2));
#8526=CARTESIAN_POINT('',(-2.2,0.2875,0.2));
#8527=CARTESIAN_POINT('',(-2.2,-0.1,0.));
#8528=CARTESIAN_POINT('',(-2.2,-0.1,0.));
#8529=CARTESIAN_POINT('',(-2.2,-0.1,0.));
#8530=CARTESIAN_POINT('Origin',(-6.4,-0.1,0.));
#8531=CARTESIAN_POINT('',(-6.4,0.0214285714285713,0.0809523809523809));
#8532=CARTESIAN_POINT('',(-5.56666666666667,0.2,0.2));
#8533=CARTESIAN_POINT('',(-5.78548644338118,0.15311004784689,0.168740031897927));
#8534=CARTESIAN_POINT('',(-6.4,-0.1,0.));
#8535=CARTESIAN_POINT('',(-6.4,-0.1,0.));
#8536=CARTESIAN_POINT('',(-2.2,-0.1,0.));
#8537=CARTESIAN_POINT('',(-5.225,0.2,0.2));
#8538=CARTESIAN_POINT('Origin',(-6.4,0.025,0.125));
#8539=CARTESIAN_POINT('',(-6.4,0.0214285714285713,0.2));
#8540=CARTESIAN_POINT('',(-6.4,0.0214285714285713,0.0625));
#8541=CARTESIAN_POINT('',(-6.4,-0.1,0.2));
#8542=CARTESIAN_POINT('',(-6.4,0.2875,0.2));
#8543=CARTESIAN_POINT('',(-6.4,-0.1,0.));
#8544=CARTESIAN_POINT('Origin',(-4.05,0.55,0.2));
#8545=CARTESIAN_POINT('',(-6.5,0.,0.2));
#8546=CARTESIAN_POINT('',(-6.5,0.,0.2));
#8547=CARTESIAN_POINT('',(-6.4,-0.1,0.2));
#8548=CARTESIAN_POINT('Origin',(-4.05,0.55,0.2));
#8549=CARTESIAN_POINT('',(-2.,0.133333333333333,0.2));
#8550=CARTESIAN_POINT('',(-1.6,0.6,0.2));
#8551=CARTESIAN_POINT('',(-2.,0.933333333333333,0.2));
#8552=CARTESIAN_POINT('',(-2.,0.875,0.2));
#8553=CARTESIAN_POINT('',(-2.5,0.6,0.2));
#8554=CARTESIAN_POINT('',(-2.5,0.6,0.2));
#8555=CARTESIAN_POINT('',(-5.1,0.3,0.2));
#8556=CARTESIAN_POINT('',(-5.1,0.3,0.2));
#8557=CARTESIAN_POINT('',(-6.5,0.,0.2));
#8558=CARTESIAN_POINT('Origin',(-1.6,1.2,0.));
#8559=CARTESIAN_POINT('',(-2.,0.933333333333333,0.));
#8560=CARTESIAN_POINT('',(-2.,0.933333333333333,0.));
#8561=CARTESIAN_POINT('',(-2.5,0.6,0.));
#8562=CARTESIAN_POINT('',(-2.5,0.6,0.));
#8563=CARTESIAN_POINT('',(-2.5,0.6,0.));
#8564=CARTESIAN_POINT('Origin',(-2.2,-0.1,0.));
#8565=CARTESIAN_POINT('',(-2.,0.133333333333333,0.));
#8566=CARTESIAN_POINT('',(-2.,0.133333333333334,0.));
#8567=CARTESIAN_POINT('',(-1.6,0.6,0.));
#8568=CARTESIAN_POINT('Origin',(-6.5,0.,0.));
#8569=CARTESIAN_POINT('',(-6.5,0.,0.));
#8570=CARTESIAN_POINT('',(-6.4,-0.1,0.));
#8571=CARTESIAN_POINT('',(-6.5,0.,0.));
#8572=CARTESIAN_POINT('Origin',(-5.1,0.3,0.));
#8573=CARTESIAN_POINT('',(-5.1,0.3,0.));
#8574=CARTESIAN_POINT('',(-5.1,0.3,0.));
#8575=CARTESIAN_POINT('',(-6.5,0.,0.));
#8576=CARTESIAN_POINT('Origin',(-2.5,0.6,0.));
#8577=CARTESIAN_POINT('',(-5.1,0.3,0.));
#8578=CARTESIAN_POINT('Origin',(0.,0.,0.));
#8579=CARTESIAN_POINT('',(-2.,1.2,0.));
#8580=CARTESIAN_POINT('',(-2.,0.,0.));
#8581=CARTESIAN_POINT('',(-1.2,1.2,0.));
#8582=CARTESIAN_POINT('',(-2.,1.2,0.));
#8583=CARTESIAN_POINT('',(-1.2,0.721110255092798,0.));
#8584=CARTESIAN_POINT('',(-1.2,1.2,0.));
#8585=CARTESIAN_POINT('',(0.993295878967653,0.986591757935306,0.));
#8586=CARTESIAN_POINT('Origin',(0.,0.,0.));
#8587=CARTESIAN_POINT('',(1.,1.,0.));
#8588=CARTESIAN_POINT('',(1.,1.,0.));
#8589=CARTESIAN_POINT('',(3.8,-1.9,0.));
#8590=CARTESIAN_POINT('',(3.8,-1.9,0.));
#8591=CARTESIAN_POINT('',(14.,-1.9,0.));
#8592=CARTESIAN_POINT('',(14.,-1.9,0.));
#8593=CARTESIAN_POINT('',(14.,-3.1,0.));
#8594=CARTESIAN_POINT('',(14.,-3.1,0.));
#8595=CARTESIAN_POINT('',(3.8,-3.1,0.));
#8596=CARTESIAN_POINT('',(3.8,-3.1,0.));
#8597=CARTESIAN_POINT('',(0.533017816115691,-1.29456247732709,0.));
#8598=CARTESIAN_POINT('',(0.,-1.,0.));
#8599=CARTESIAN_POINT('',(-1.4,0.,0.));
#8600=CARTESIAN_POINT('Origin',(0.,0.,0.));
#8601=CARTESIAN_POINT('',(-2.,0.,0.));
#8602=CARTESIAN_POINT('',(-1.2,0.,0.));
#8603=CARTESIAN_POINT('',(-2.,0.,0.));
#8604=CARTESIAN_POINT('Origin',(-2.,0.,0.));
#8605=CARTESIAN_POINT('',(-1.4,0.,0.6));
#8606=CARTESIAN_POINT('',(-1.4,0.,0.));
#8607=CARTESIAN_POINT('',(-2.,0.,0.6));
#8608=CARTESIAN_POINT('',(-1.2,0.,0.6));
#8609=CARTESIAN_POINT('',(-2.,0.,0.));
#8610=CARTESIAN_POINT('Origin',(-2.,1.2,0.));
#8611=CARTESIAN_POINT('',(-2.,1.2,0.6));
#8612=CARTESIAN_POINT('',(-2.,0.,0.6));
#8613=CARTESIAN_POINT('',(-2.,1.2,0.));
#8614=CARTESIAN_POINT('Origin',(-1.2,1.2,0.));
#8615=CARTESIAN_POINT('',(-1.2,1.2,0.6));
#8616=CARTESIAN_POINT('',(-2.,1.2,0.6));
#8617=CARTESIAN_POINT('',(-1.2,1.2,0.));
#8618=CARTESIAN_POINT('Origin',(-1.2,0.,0.));
#8619=CARTESIAN_POINT('',(-1.2,0.721110255092798,0.6));
#8620=CARTESIAN_POINT('',(-1.2,0.721110255092798,0.));
#8621=CARTESIAN_POINT('',(-1.2,1.2,0.6));
#8622=CARTESIAN_POINT('Origin',(0.,0.,0.));
#8623=CARTESIAN_POINT('',(0.533017816115691,-1.29456247732709,0.6));
#8624=CARTESIAN_POINT('',(0.533017816115691,-1.29456247732709,0.));
#8625=CARTESIAN_POINT('Origin',(0.,0.,0.6));
#8626=CARTESIAN_POINT('Origin',(0.,0.,0.));
#8627=CARTESIAN_POINT('',(0.993295878967653,0.986591757935306,0.6));
#8628=CARTESIAN_POINT('Origin',(0.,0.,0.6));
#8629=CARTESIAN_POINT('',(0.993295878967653,0.986591757935306,0.));
#8630=CARTESIAN_POINT('Origin',(0.,0.,0.6));
#8631=CARTESIAN_POINT('',(3.8,-3.1,0.6));
#8632=CARTESIAN_POINT('',(0.,-1.,0.6));
#8633=CARTESIAN_POINT('',(14.,-3.1,0.6));
#8634=CARTESIAN_POINT('',(3.8,-3.1,0.6));
#8635=CARTESIAN_POINT('',(14.,-1.9,0.6));
#8636=CARTESIAN_POINT('',(14.,-3.1,0.6));
#8637=CARTESIAN_POINT('',(3.8,-1.9,0.6));
#8638=CARTESIAN_POINT('',(14.,-1.9,0.6));
#8639=CARTESIAN_POINT('',(1.,1.,0.6));
#8640=CARTESIAN_POINT('',(3.8,-1.9,0.6));
#8641=CARTESIAN_POINT('',(1.,1.,0.6));
#8642=CARTESIAN_POINT('Origin',(0.,-1.,0.));
#8643=CARTESIAN_POINT('',(3.8,-3.1,0.));
#8644=CARTESIAN_POINT('Origin',(1.,1.,0.));
#8645=CARTESIAN_POINT('',(1.,1.,0.));
#8646=CARTESIAN_POINT('Origin',(3.8,-1.9,0.));
#8647=CARTESIAN_POINT('',(3.8,-1.9,0.));
#8648=CARTESIAN_POINT('Origin',(14.,-1.9,0.));
#8649=CARTESIAN_POINT('',(14.,-1.9,0.));
#8650=CARTESIAN_POINT('Origin',(14.,-3.1,0.));
#8651=CARTESIAN_POINT('',(14.,-3.1,0.));
#8652=CARTESIAN_POINT('Origin',(3.8,-3.1,0.));
#8653=CARTESIAN_POINT('',(0.,0.,0.));
#8654=CARTESIAN_POINT('Origin',(0.,0.,0.75));
#8655=CARTESIAN_POINT('',(-0.3,-3.67394039744206E-17,0.7));
#8656=CARTESIAN_POINT('Origin',(0.,0.,0.7));
#8657=CARTESIAN_POINT('',(-0.3,-3.67394039744206E-17,0.8));
#8658=CARTESIAN_POINT('',(-0.3,-3.67394039744206E-17,0.75));
#8659=CARTESIAN_POINT('Origin',(0.,0.,0.8));
#8660=CARTESIAN_POINT('Origin',(0.7,0.,0.7));
#8661=CARTESIAN_POINT('',(-0.4,4.89858719658941E-17,0.7));
#8662=CARTESIAN_POINT('Origin',(0.,0.,0.7));
#8663=CARTESIAN_POINT('Origin',(0.3,0.,0.8));
#8664=CARTESIAN_POINT('',(-0.4,-4.89858719658941E-17,0.8));
#8665=CARTESIAN_POINT('Origin',(0.,0.,0.8));
#8666=CARTESIAN_POINT('Origin',(0.,0.,-0.7));
#8667=CARTESIAN_POINT('',(-0.4,-4.89858719658941E-17,0.9));
#8668=CARTESIAN_POINT('Origin',(0.,0.,0.9));
#8669=CARTESIAN_POINT('',(-0.4,-4.89858719658941E-17,-0.7));
#8670=CARTESIAN_POINT('Origin',(0.,0.,-0.7));
#8671=CARTESIAN_POINT('',(-0.6,-7.34788079488412E-17,-0.7));
#8672=CARTESIAN_POINT('Origin',(0.,0.,-0.7));
#8673=CARTESIAN_POINT('',(-0.4,-4.89858719658941E-17,-0.7));
#8674=CARTESIAN_POINT('Origin',(0.,0.,-0.7));
#8675=CARTESIAN_POINT('Origin',(0.,0.,-0.8));
#8676=CARTESIAN_POINT('',(-0.6,-7.34788079488412E-17,-0.8));
#8677=CARTESIAN_POINT('',(-0.6,-7.34788079488412E-17,-0.8));
#8678=CARTESIAN_POINT('Origin',(0.,0.,-0.8));
#8679=CARTESIAN_POINT('Origin',(0.,0.,-0.8));
#8680=CARTESIAN_POINT('Origin',(0.,0.,-0.7));
#8681=CARTESIAN_POINT('',(-0.4,-4.89858719658941E-17,-0.7));
#8682=CARTESIAN_POINT('Origin',(0.,0.,0.9));
#8683=CARTESIAN_POINT('',(0.,0.,0.));
#8684=CARTESIAN_POINT('Origin',(-0.1,0.,0.1));
#8685=CARTESIAN_POINT('',(-0.1,0.282842712474619,0.));
#8686=CARTESIAN_POINT('',(-0.1,0.282842712474619,0.1));
#8687=CARTESIAN_POINT('',(-0.1,0.282842712474619,0.));
#8688=CARTESIAN_POINT('',(-0.1,0.591607978309962,0.));
#8689=CARTESIAN_POINT('',(-0.1,0.,0.));
#8690=CARTESIAN_POINT('',(-0.1,0.591607978309962,0.1));
#8691=CARTESIAN_POINT('',(-0.1,0.591607978309962,0.));
#8692=CARTESIAN_POINT('',(-0.1,0.,0.1));
#8693=CARTESIAN_POINT('Origin',(0.1,1.2,0.1));
#8694=CARTESIAN_POINT('',(0.1,0.282842712474619,0.1));
#8695=CARTESIAN_POINT('',(0.1,0.282842712474619,0.));
#8696=CARTESIAN_POINT('',(0.1,0.282842712474619,0.));
#8697=CARTESIAN_POINT('',(0.1,0.591607978309962,0.1));
#8698=CARTESIAN_POINT('',(0.1,0.6,0.1));
#8699=CARTESIAN_POINT('',(0.1,0.591607978309962,0.));
#8700=CARTESIAN_POINT('',(0.1,0.591607978309962,0.));
#8701=CARTESIAN_POINT('',(0.1,0.6,0.));
#8702=CARTESIAN_POINT('Origin',(0.,0.,0.));
#8703=CARTESIAN_POINT('Origin',(0.,0.,0.));
#8704=CARTESIAN_POINT('Origin',(0.,0.,0.));
#8705=CARTESIAN_POINT('Origin',(0.,0.,0.));
#8706=CARTESIAN_POINT('Origin',(0.,0.,0.1));
#8707=CARTESIAN_POINT('Origin',(0.,0.,0.));
#8708=CARTESIAN_POINT('Origin',(0.,0.,0.1));
#8709=CARTESIAN_POINT('Origin',(0.,0.,0.1));
#8710=CARTESIAN_POINT('',(0.,0.,0.));
#8711=CARTESIAN_POINT('',(0.,0.,0.));
#8712=CARTESIAN_POINT('Origin',(8.1,-1.,0.7));
#8713=CARTESIAN_POINT('',(7.94916965151797,-1.19937453693185,0.7));
#8714=CARTESIAN_POINT('',(8.26514540988519,-1.18768855477586,0.7));
#8715=CARTESIAN_POINT('Ctrl Pts',(7.94916965151797,-1.19937453693185,0.7));
#8716=CARTESIAN_POINT('Ctrl Pts',(7.97160858810976,-1.21634998764782,0.7));
#8717=CARTESIAN_POINT('Ctrl Pts',(7.99739856866269,-1.22989011121344,0.69528529300377));
#8718=CARTESIAN_POINT('Ctrl Pts',(8.03944443766207,-1.24298414277179,0.688517705185315));
#8719=CARTESIAN_POINT('Ctrl Pts',(8.05362924383607,-1.24609346022897,0.686388676887586));
#8720=CARTESIAN_POINT('Ctrl Pts',(8.075506183533,-1.24890990228851,0.684139035126277));
#8721=CARTESIAN_POINT('Ctrl Pts',(8.08297567221474,-1.24953307703463,0.683546226354886));
#8722=CARTESIAN_POINT('Ctrl Pts',(8.0940066533036,-1.24995288972095,0.68299521602547));
#8723=CARTESIAN_POINT('Ctrl Pts',(8.09752287926269,-1.25001251279495,0.68286729538075));
#8724=CARTESIAN_POINT('Ctrl Pts',(8.10293413375911,-1.249989933108,0.682747340264197));
#8725=CARTESIAN_POINT('Ctrl Pts',(8.10482478940148,-1.24996059450444,0.682719828470948));
#8726=CARTESIAN_POINT('Ctrl Pts',(8.10828546792054,-1.24986760009171,0.682696100760705));
#8727=CARTESIAN_POINT('Ctrl Pts',(8.10985478687837,-1.24981062779486,0.682695370268813));
#8728=CARTESIAN_POINT('Ctrl Pts',(8.11326464342549,-1.24965465239671,0.682715595753076));
#8729=CARTESIAN_POINT('Ctrl Pts',(8.11510409202247,-1.2495501177419,0.682740330911594));
#8730=CARTESIAN_POINT('Ctrl Pts',(8.12014207260669,-1.24920790966494,0.682845651127781));
#8731=CARTESIAN_POINT('Ctrl Pts',(8.12333423895876,-1.24892926854386,0.682953992816581));
#8732=CARTESIAN_POINT('Ctrl Pts',(8.139194120874,-1.2472372768871,0.683691668462565));
#8733=CARTESIAN_POINT('Ctrl Pts',(8.15164141295685,-1.2449338270761,0.684918799511701));
#8734=CARTESIAN_POINT('Ctrl Pts',(8.19196937649467,-1.23428099896052,0.690212518998986));
#8735=CARTESIAN_POINT('Ctrl Pts',(8.21811504697062,-1.22213176592155,0.695755006185672));
#8736=CARTESIAN_POINT('Ctrl Pts',(8.24962874265135,-1.20052913769617,0.699397421419897));
#8737=CARTESIAN_POINT('Ctrl Pts',(8.25758631484639,-1.19433973204149,0.7));
#8738=CARTESIAN_POINT('Ctrl Pts',(8.26514540988519,-1.18768855477586,0.7));
#8739=CARTESIAN_POINT('Origin',(8.1,-1.,0.7));
#8740=CARTESIAN_POINT('Origin',(2.7,1.,0.7));
#8741=CARTESIAN_POINT('',(2.8076286513348,1.22564590451442,0.7));
#8742=CARTESIAN_POINT('',(2.57739843082973,1.21787348447435,0.7));
#8743=CARTESIAN_POINT('Ctrl Pts',(2.80762864495888,1.22564590575571,0.7));
#8744=CARTESIAN_POINT('Ctrl Pts',(2.78743249310418,1.23527907171202,0.7));
#8745=CARTESIAN_POINT('Ctrl Pts',(2.76507271635938,1.24261561512899,0.698430289974852));
#8746=CARTESIAN_POINT('Ctrl Pts',(2.73219941643314,1.24807722603274,0.696876198609429));
#8747=CARTESIAN_POINT('Ctrl Pts',(2.72335305886828,1.24906618730719,0.696525251810408));
#8748=CARTESIAN_POINT('Ctrl Pts',(2.71018695034311,1.24982905432238,0.696188910804419));
#8749=CARTESIAN_POINT('Ctrl Pts',(2.70590779780308,1.24996687586326,0.696107915309552));
#8750=CARTESIAN_POINT('Ctrl Pts',(2.69921702211412,1.25001037316246,0.696030339680738));
#8751=CARTESIAN_POINT('Ctrl Pts',(2.69680890442544,1.24999123464332,0.696012302673685));
#8752=CARTESIAN_POINT('Ctrl Pts',(2.69234597975348,1.24989125947742,0.695997601992606));
#8753=CARTESIAN_POINT('Ctrl Pts',(2.69029169500035,1.24981988388707,0.69599819279703));
#8754=CARTESIAN_POINT('Ctrl Pts',(2.6857660481318,1.24960673159635,0.696015705561832));
#8755=CARTESIAN_POINT('Ctrl Pts',(2.68329599580702,1.24945360531346,0.696035938105249));
#8756=CARTESIAN_POINT('Ctrl Pts',(2.67625328071593,1.24891193026541,0.696123377063474));
#8757=CARTESIAN_POINT('Ctrl Pts',(2.67169109188753,1.24843439216159,0.696216059649547));
#8758=CARTESIAN_POINT('Ctrl Pts',(2.64765560351845,1.24524789167778,0.696873729305584));
#8759=CARTESIAN_POINT('Ctrl Pts',(2.62857598726268,1.24037162800668,0.698048768812303));
#8760=CARTESIAN_POINT('Ctrl Pts',(2.59902076831046,1.22902239593109,0.699541037747764));
#8761=CARTESIAN_POINT('Ctrl Pts',(2.58799157881597,1.22383445108162,0.7));
#8762=CARTESIAN_POINT('Ctrl Pts',(2.57739843082979,1.21787348447436,0.7));
#8763=CARTESIAN_POINT('Origin',(2.7,1.,0.7));
#8764=CARTESIAN_POINT('Origin',(2.7,-1.,0.7));
#8765=CARTESIAN_POINT('',(2.57739843082979,-1.21787348447436,0.7));
#8766=CARTESIAN_POINT('',(2.80762864495888,-1.22564590575571,0.7));
#8767=CARTESIAN_POINT('Ctrl Pts',(2.57739843082979,-1.21787348447436,0.7));
#8768=CARTESIAN_POINT('Ctrl Pts',(2.59689796709118,-1.22884624579732,0.7));
#8769=CARTESIAN_POINT('Ctrl Pts',(2.61871070177046,-1.23767364961455,0.698430520021629));
#8770=CARTESIAN_POINT('Ctrl Pts',(2.6511387549791,-1.24533993869645,0.696876447160353));
#8771=CARTESIAN_POINT('Ctrl Pts',(2.65989793055836,-1.24692336726652,0.696525471319567));
#8772=CARTESIAN_POINT('Ctrl Pts',(2.67298219502323,-1.24857266139659,0.696189053183015));
#8773=CARTESIAN_POINT('Ctrl Pts',(2.67724223626036,-1.24899884484677,0.696108027479433));
#8774=CARTESIAN_POINT('Ctrl Pts',(2.68391475503581,-1.24949361628703,0.696030400846995));
#8775=CARTESIAN_POINT('Ctrl Pts',(2.68631866330158,-1.24963697932539,0.69601234479389));
#8776=CARTESIAN_POINT('Ctrl Pts',(2.69077815115796,-1.24983831390468,0.695997608323079));
#8777=CARTESIAN_POINT('Ctrl Pts',(2.69283257145917,-1.24990568929416,0.695998182544699));
#8778=CARTESIAN_POINT('Ctrl Pts',(2.69736230434386,-1.24999833696454,0.696015659042177));
#8779=CARTESIAN_POINT('Ctrl Pts',(2.69983707579759,-1.25001219669429,0.696035872086962));
#8780=CARTESIAN_POINT('Ctrl Pts',(2.70690037992806,-1.24994687665095,0.696123257636812));
#8781=CARTESIAN_POINT('Ctrl Pts',(2.71148446565418,-1.24977820005943,0.696215908504701));
#8782=CARTESIAN_POINT('Ctrl Pts',(2.73568105999059,-1.24822038288304,0.696873447340259));
#8783=CARTESIAN_POINT('Ctrl Pts',(2.75504695022812,-1.24464213141243,0.698048515307351));
#8784=CARTESIAN_POINT('Ctrl Pts',(2.78530198112344,-1.2353118289445,0.699540950501024));
#8785=CARTESIAN_POINT('Ctrl Pts',(2.79665680001786,-1.23087925931356,0.7));
#8786=CARTESIAN_POINT('Ctrl Pts',(2.80762864495888,-1.22564590575571,0.7));
#8787=CARTESIAN_POINT('Origin',(2.7,-1.,0.7));
#8788=CARTESIAN_POINT('Origin',(8.1,1.,0.7));
#8789=CARTESIAN_POINT('',(8.26514540988519,1.18768855477586,0.7));
#8790=CARTESIAN_POINT('',(7.94916965249954,1.19937453719419,0.7));
#8791=CARTESIAN_POINT('Ctrl Pts',(8.26514540988519,1.18768855477586,0.7));
#8792=CARTESIAN_POINT('Ctrl Pts',(8.24402114884725,1.20627559516199,0.7));
#8793=CARTESIAN_POINT('Ctrl Pts',(8.21930102059268,1.22168408824046,0.695284768760077));
#8794=CARTESIAN_POINT('Ctrl Pts',(8.17833936508797,1.23784683595578,0.688517484674842));
#8795=CARTESIAN_POINT('Ctrl Pts',(8.16442627443898,1.24199461640617,0.686388979601913));
#8796=CARTESIAN_POINT('Ctrl Pts',(8.14282164862934,1.24641910835203,0.684139556285851));
#8797=CARTESIAN_POINT('Ctrl Pts',(8.13541969045672,1.24759243465272,0.683546718614312));
#8798=CARTESIAN_POINT('Ctrl Pts',(8.12445132655127,1.24882623938238,0.682995554842566));
#8799=CARTESIAN_POINT('Ctrl Pts',(8.12094947916695,1.24914555886372,0.68286756899844));
#8800=CARTESIAN_POINT('Ctrl Pts',(8.11555178799172,1.24952297970176,0.682747494033431));
#8801=CARTESIAN_POINT('Ctrl Pts',(8.11366421100955,1.24963346420394,0.682719937279798));
#8802=CARTESIAN_POINT('Ctrl Pts',(8.11020620287515,1.24979651712922,0.682696124556263));
#8803=CARTESIAN_POINT('Ctrl Pts',(8.10863696767328,1.24985569708818,0.682695355189016));
#8804=CARTESIAN_POINT('Ctrl Pts',(8.10522484403353,1.249952190393,0.682715496638402));
#8805=CARTESIAN_POINT('Ctrl Pts',(8.10338263267786,1.24998390529834,0.682740187713169));
#8806=CARTESIAN_POINT('Ctrl Pts',(8.09833277498968,1.25001501472208,0.682845394223802));
#8807=CARTESIAN_POINT('Ctrl Pts',(8.09512844909059,1.24997307323179,0.682953673497893));
#8808=CARTESIAN_POINT('Ctrl Pts',(8.07918314804204,1.24945780552822,0.683691186949858));
#8809=CARTESIAN_POINT('Ctrl Pts',(8.06659630270856,1.24808001426183,0.684918585227095));
#8810=CARTESIAN_POINT('Ctrl Pts',(8.02558960427868,1.24043495378573,0.69021260546313));
#8811=CARTESIAN_POINT('Ctrl Pts',(7.9986188553413,1.2302509517108,0.695754623970086));
#8812=CARTESIAN_POINT('Ctrl Pts',(7.96559475436581,1.21103543221342,0.69939729083119));
#8813=CARTESIAN_POINT('Ctrl Pts',(7.95720051358587,1.20545002552208,0.7));
#8814=CARTESIAN_POINT('Ctrl Pts',(7.94916965151797,1.19937453693185,0.7));
#8815=CARTESIAN_POINT('Origin',(8.1,1.,0.7));
#8816=CARTESIAN_POINT('Ctrl Pts',(1.1,1.14549341399196,0.7));
#8817=CARTESIAN_POINT('Ctrl Pts',(1.89984199608574,1.1957170361627,0.7));
#8818=CARTESIAN_POINT('Ctrl Pts',(2.70080437300401,1.2273695200909,0.7));
#8819=CARTESIAN_POINT('Ctrl Pts',(3.50204003610941,1.24374118183538,0.7));
#8820=CARTESIAN_POINT('Ctrl Pts',(1.09819048660397,1.17431102498992,0.7));
#8821=CARTESIAN_POINT('Ctrl Pts',(1.89847848223077,1.22458382597074,0.70000077422621));
#8822=CARTESIAN_POINT('Ctrl Pts',(2.69984520196781,1.25626413437997,0.699999727319846));
#8823=CARTESIAN_POINT('Ctrl Pts',(3.50144932661635,1.27265074030048,0.700000000000001));
#8824=CARTESIAN_POINT('Ctrl Pts',(1.09505363188407,1.22426736091617,0.676703190608825));
#8825=CARTESIAN_POINT('Ctrl Pts',(1.89610976425884,1.27462253270773,0.67666760713801));
#8826=CARTESIAN_POINT('Ctrl Pts',(2.69818680938115,1.3063522351595,0.67664530655333));
#8827=CARTESIAN_POINT('Ctrl Pts',(3.50042536655637,1.322763754511,0.676632802377821));
#8828=CARTESIAN_POINT('Ctrl Pts',(1.09381704710221,1.24396073223232,0.627109609335854));
#8829=CARTESIAN_POINT('Ctrl Pts',(1.89518106151152,1.29430885982199,0.62701751976321));
#8830=CARTESIAN_POINT('Ctrl Pts',(2.69753328610131,1.32603127467068,0.626959208652505));
#8831=CARTESIAN_POINT('Ctrl Pts',(3.50002334924346,1.34243864233338,0.626926882269943));
#8832=CARTESIAN_POINT('Ctrl Pts',(1.09374258853658,1.24514653057163,0.605486452199395));
#8833=CARTESIAN_POINT('Ctrl Pts',(1.89512529323683,1.29547288309274,0.605377720397184));
#8834=CARTESIAN_POINT('Ctrl Pts',(2.69749615303001,1.32718177535833,0.605308474776761));
#8835=CARTESIAN_POINT('Ctrl Pts',(3.5,1.34358136363184,0.605270327458635));
#8836=CARTESIAN_POINT('',(1.1,1.14549341399195,0.7));
#8837=CARTESIAN_POINT('Ctrl Pts',(1.1,1.14549341399196,0.7));
#8838=CARTESIAN_POINT('Ctrl Pts',(1.59210562457523,1.17639367564078,0.7));
#8839=CARTESIAN_POINT('Ctrl Pts',(2.08463535466703,1.20026407570248,0.7));
#8840=CARTESIAN_POINT('Ctrl Pts',(2.57739190516306,1.2178709162388,0.7));
#8841=CARTESIAN_POINT('',(1.1,1.24553911298206,0.605485603995113));
#8842=CARTESIAN_POINT('Ctrl Pts',(1.1,1.14549341399196,0.7));
#8843=CARTESIAN_POINT('Ctrl Pts',(1.1,1.15341616150799,0.7));
#8844=CARTESIAN_POINT('Ctrl Pts',(1.1000012416168,1.16127613060545,0.699006361583129));
#8845=CARTESIAN_POINT('Ctrl Pts',(1.10000231308998,1.16893252943985,0.697119293189023));
#8846=CARTESIAN_POINT('Ctrl Pts',(1.10000291357081,1.17322337016277,0.696061732044743));
#8847=CARTESIAN_POINT('Ctrl Pts',(1.10000345673767,1.17745032641463,0.694722535963768));
#8848=CARTESIAN_POINT('Ctrl Pts',(1.10000379529503,1.18158693416151,0.693112479763539));
#8849=CARTESIAN_POINT('Ctrl Pts',(1.1000044034764,1.18901789868739,0.690220189452084));
#8850=CARTESIAN_POINT('Ctrl Pts',(1.1000042334852,1.19607766167095,0.686488065947256));
#8851=CARTESIAN_POINT('Ctrl Pts',(1.10000339376692,1.2026196529327,0.681996646156542));
#8852=CARTESIAN_POINT('Ctrl Pts',(1.10000293249552,1.20621327895058,0.67952943359521));
#8853=CARTESIAN_POINT('Ctrl Pts',(1.10000228571683,1.20965039763183,0.676832226278619));
#8854=CARTESIAN_POINT('Ctrl Pts',(1.10000171524363,1.21290279159005,0.673912896410569));
#8855=CARTESIAN_POINT('Ctrl Pts',(1.10000115816795,1.2160788033717,0.671062126739188));
#8856=CARTESIAN_POINT('Ctrl Pts',(1.10000066850715,1.2190594221245,0.668016750164662));
#8857=CARTESIAN_POINT('Ctrl Pts',(1.10000067525152,1.22182202639256,0.664788091882127));
#8858=CARTESIAN_POINT('Ctrl Pts',(1.10000068775799,1.22694487635592,0.658801012170571));
#8859=CARTESIAN_POINT('Ctrl Pts',(1.10000222199399,1.23132099043293,0.652185071179834));
#8860=CARTESIAN_POINT('Ctrl Pts',(1.10000276904041,1.23488987417606,0.64510534613808));
#8861=CARTESIAN_POINT('Ctrl Pts',(1.10000282439334,1.23525099193115,0.644388983656765));
#8862=CARTESIAN_POINT('Ctrl Pts',(1.10000287212626,1.23560380546488,0.64366785367332));
#8863=CARTESIAN_POINT('Ctrl Pts',(1.10000291138002,1.23594822450451,0.642942116631622));
#8864=CARTESIAN_POINT('Ctrl Pts',(1.10000329911404,1.23935026814133,0.635773555081239));
#8865=CARTESIAN_POINT('Ctrl Pts',(1.10000258010782,1.24189771450306,0.628240464257889));
#8866=CARTESIAN_POINT('Ctrl Pts',(1.10000149084855,1.24353681278199,0.620511076118615));
#8867=CARTESIAN_POINT('Ctrl Pts',(1.10000079446814,1.24458471384188,0.615569557890241));
#8868=CARTESIAN_POINT('Ctrl Pts',(1.10000000111128,1.24526049271905,0.610547146027233));
#8869=CARTESIAN_POINT('Ctrl Pts',(1.09999999916631,1.24553911263843,0.605485603997432));
#8870=CARTESIAN_POINT('',(3.5,1.34358136363184,0.605270327458635));
#8871=CARTESIAN_POINT('Ctrl Pts',(3.5,1.34358136363184,0.605270327458635));
#8872=CARTESIAN_POINT('Ctrl Pts',(2.6995848679345,1.32722445934619,0.605308375488923));
#8873=CARTESIAN_POINT('Ctrl Pts',(1.89930203168261,1.29563783986497,0.605377360150118));
#8874=CARTESIAN_POINT('Ctrl Pts',(1.09999999916631,1.24553911263843,0.605485603997431));
#8875=CARTESIAN_POINT('',(3.5,1.24369946473792,0.7));
#8876=CARTESIAN_POINT('Ctrl Pts',(3.5,1.34358136363184,0.605270327458635));
#8877=CARTESIAN_POINT('Ctrl Pts',(3.5,1.34316359984937,0.613184373088104));
#8878=CARTESIAN_POINT('Ctrl Pts',(3.50000057901142,1.34177887744868,0.621008021569537));
#8879=CARTESIAN_POINT('Ctrl Pts',(3.50000082863025,1.33951086762262,0.628580534231506));
#8880=CARTESIAN_POINT('Ctrl Pts',(3.50000096811,1.33824356956914,0.632811834486987));
#8881=CARTESIAN_POINT('Ctrl Pts',(3.50000102536574,1.33669948631919,0.636964759527324));
#8882=CARTESIAN_POINT('Ctrl Pts',(3.50000098105742,1.334886463945,0.641009258704104));
#8883=CARTESIAN_POINT('Ctrl Pts',(3.50000090179773,1.3316432906201,0.648244145614236));
#8884=CARTESIAN_POINT('Ctrl Pts',(3.50000044940971,1.3275777080273,0.655054131048541));
#8885=CARTESIAN_POINT('Ctrl Pts',(3.50000027423476,1.32275302640998,0.661275670751788));
#8886=CARTESIAN_POINT('Ctrl Pts',(3.50000024156065,1.32185311357394,0.66243612938574));
#8887=CARTESIAN_POINT('Ctrl Pts',(3.50000022115524,1.32092666334894,0.663576045687695));
#8888=CARTESIAN_POINT('Ctrl Pts',(3.50000022069074,1.31997391848392,0.664694242102532));
#8889=CARTESIAN_POINT('Ctrl Pts',(3.50000021976176,1.31806844339147,0.666930617752677));
#8890=CARTESIAN_POINT('Ctrl Pts',(3.50000029790302,1.31605782519,0.669080165434128));
#8891=CARTESIAN_POINT('Ctrl Pts',(3.50000040488465,1.31394946763378,0.671139079687271));
#8892=CARTESIAN_POINT('Ctrl Pts',(3.50000069329649,1.3082655455861,0.6766897075128));
#8893=CARTESIAN_POINT('Ctrl Pts',(3.5000011432336,1.30193818666762,0.681521899278667));
#8894=CARTESIAN_POINT('Ctrl Pts',(3.50000129797765,1.29513115062548,0.68558123547136));
#8895=CARTESIAN_POINT('Ctrl Pts',(3.50000139624096,1.2908086457691,0.688158936000333));
#8896=CARTESIAN_POINT('Ctrl Pts',(3.50000139493488,1.28629176508013,0.690424313967808));
#8897=CARTESIAN_POINT('Ctrl Pts',(3.50000129141552,1.28161680488022,0.692354162840695));
#8898=CARTESIAN_POINT('Ctrl Pts',(3.50000112941005,1.27430059661786,0.695374333209024));
#8899=CARTESIAN_POINT('Ctrl Pts',(3.5000007162179,1.26668229982361,0.697540280949125));
#8900=CARTESIAN_POINT('Ctrl Pts',(3.50000038344698,1.25890895215876,0.698782355543395));
#8901=CARTESIAN_POINT('Ctrl Pts',(3.50000016866387,1.25389173534334,0.699584038140014));
#8902=CARTESIAN_POINT('Ctrl Pts',(3.4999999993056,1.24880933504677,0.69999999987784));
#8903=CARTESIAN_POINT('Ctrl Pts',(3.49999999991873,1.24369946470729,0.7));
#8904=CARTESIAN_POINT('Ctrl Pts',(2.80762377174497,1.22564400643366,0.7));
#8905=CARTESIAN_POINT('Ctrl Pts',(3.03837960601223,1.23298334400942,0.7));
#8906=CARTESIAN_POINT('Ctrl Pts',(3.26917843294065,1.23897560812206,0.7));
#8907=CARTESIAN_POINT('Ctrl Pts',(3.49999999991873,1.24369946470729,0.7));
#8908=CARTESIAN_POINT('Ctrl Pts',(7.29709043526678,1.22049830417059,0.7));
#8909=CARTESIAN_POINT('Ctrl Pts',(8.19846709497879,1.19422430779862,0.7));
#8910=CARTESIAN_POINT('Ctrl Pts',(9.09944331332256,1.15544418981837,0.7));
#8911=CARTESIAN_POINT('Ctrl Pts',(10.,1.10900986674273,0.7));
#8912=CARTESIAN_POINT('Ctrl Pts',(7.29793284700474,1.24939875264889,0.7));
#8913=CARTESIAN_POINT('Ctrl Pts',(8.19957769811722,1.22310890030201,0.699999704549177));
#8914=CARTESIAN_POINT('Ctrl Pts',(9.10076698492607,1.18430758604571,0.700000491839571));
#8915=CARTESIAN_POINT('Ctrl Pts',(10.0014871213396,1.13785139984992,0.7));
#8916=CARTESIAN_POINT('Ctrl Pts',(7.29939288958794,1.29948813715084,0.676630595533454));
#8917=CARTESIAN_POINT('Ctrl Pts',(8.20149954052228,1.27317186922949,0.676644146017132));
#8918=CARTESIAN_POINT('Ctrl Pts',(9.10306300621911,1.23433322993607,0.676664155483857));
#8919=CARTESIAN_POINT('Ctrl Pts',(10.0040646682326,1.18784086746588,0.676686753673613));
#8920=CARTESIAN_POINT('Ctrl Pts',(7.29996660609513,1.31917051289423,0.626939603849942));
#8921=CARTESIAN_POINT('Ctrl Pts',(8.20225661204673,1.29285896783792,0.626974637782525));
#8922=CARTESIAN_POINT('Ctrl Pts',(9.10396596140606,1.25402923300358,0.627026849623412));
#8923=CARTESIAN_POINT('Ctrl Pts',(10.0050807923581,1.20754778500352,0.627085325222079));
#8924=CARTESIAN_POINT('Ctrl Pts',(7.29999999953093,1.32031613471704,0.605285370449856));
#8925=CARTESIAN_POINT('Ctrl Pts',(8.20230020786565,1.29401302889245,0.605326714446839));
#8926=CARTESIAN_POINT('Ctrl Pts',(9.10401978846669,1.25519559703033,0.605388684776982));
#8927=CARTESIAN_POINT('Ctrl Pts',(10.0051416645797,1.20872835322339,0.605457722909465));
#8928=CARTESIAN_POINT('',(7.29999999989017,1.22041345054104,0.7));
#8929=CARTESIAN_POINT('Ctrl Pts',(7.29999999978094,1.22041345055303,0.7));
#8930=CARTESIAN_POINT('Ctrl Pts',(7.51641201913776,1.21409884615949,0.7));
#8931=CARTESIAN_POINT('Ctrl Pts',(7.73280095443524,1.20706364503479,0.7));
#8932=CARTESIAN_POINT('Ctrl Pts',(7.94916654146952,1.19937499621344,0.7));
#8933=CARTESIAN_POINT('',(7.29999999953133,1.3203161347307,0.605285370449834));
#8934=CARTESIAN_POINT('Ctrl Pts',(7.29999999989087,1.22041345054982,0.7));
#8935=CARTESIAN_POINT('Ctrl Pts',(7.30000000079355,1.22832360919786,0.699999999740221));
#8936=CARTESIAN_POINT('Ctrl Pts',(7.29999941101664,1.23617007614594,0.699006006469939));
#8937=CARTESIAN_POINT('Ctrl Pts',(7.29999889581476,1.24381267896118,0.697118889344366));
#8938=CARTESIAN_POINT('Ctrl Pts',(7.29999860583198,1.24811433880851,0.696056720321257));
#8939=CARTESIAN_POINT('Ctrl Pts',(7.29999834128398,1.25235147078274,0.694710570513598));
#8940=CARTESIAN_POINT('Ctrl Pts',(7.29999817264931,1.25649739217805,0.693091458416622));
#8941=CARTESIAN_POINT('Ctrl Pts',(7.29999787070862,1.26392067210813,0.690192435210923));
#8942=CARTESIAN_POINT('Ctrl Pts',(7.29999793286912,1.27097116792553,0.686452948287278));
#8943=CARTESIAN_POINT('Ctrl Pts',(7.2999983123982,1.27750284616821,0.681954753865011));
#8944=CARTESIAN_POINT('Ctrl Pts',(7.2999985213788,1.28109939299731,0.679477906983553));
#8945=CARTESIAN_POINT('Ctrl Pts',(7.29999881895966,1.28453837241868,0.676770138671336));
#8946=CARTESIAN_POINT('Ctrl Pts',(7.29999908362886,1.28779148632494,0.673839551409954));
#8947=CARTESIAN_POINT('Ctrl Pts',(7.29999934163235,1.29096267037196,0.670982771155867));
#8948=CARTESIAN_POINT('Ctrl Pts',(7.29999957112158,1.2939379836903,0.667931525418885));
#8949=CARTESIAN_POINT('Ctrl Pts',(7.29999957127586,1.29669488996436,0.664697318929259));
#8950=CARTESIAN_POINT('Ctrl Pts',(7.29999957156178,1.30180432468448,0.658703293276094));
#8951=CARTESIAN_POINT('Ctrl Pts',(7.29999886995656,1.30616650855536,0.652082235935803));
#8952=CARTESIAN_POINT('Ctrl Pts',(7.29999863193158,1.30972187224872,0.644999691185358));
#8953=CARTESIAN_POINT('Ctrl Pts',(7.29999860759325,1.31008541227461,0.644275492840527));
#8954=CARTESIAN_POINT('Ctrl Pts',(7.29999858692673,1.31044047656777,0.643546449710686));
#8955=CARTESIAN_POINT('Ctrl Pts',(7.29999857034625,1.31078697300061,0.642812727646596));
#8956=CARTESIAN_POINT('Ctrl Pts',(7.29999840819729,1.31417553742296,0.635637287305567));
#8957=CARTESIAN_POINT('Ctrl Pts',(7.29999876577208,1.31670951795567,0.628098908385918));
#8958=CARTESIAN_POINT('Ctrl Pts',(7.29999928780719,1.3183355664444,0.620365998324013));
#8959=CARTESIAN_POINT('Ctrl Pts',(7.29999962266353,1.3193785856694,0.615405768714856));
#8960=CARTESIAN_POINT('Ctrl Pts',(7.3,1.32004717656055,0.610364828659741));
#8961=CARTESIAN_POINT('Ctrl Pts',(7.3,1.32031613470337,0.605285370449877));
#8962=CARTESIAN_POINT('',(10.,1.20899340483173,0.605457329065657));
#8963=CARTESIAN_POINT('Ctrl Pts',(9.99999999968202,1.20899340489109,0.605457329065633));
#8964=CARTESIAN_POINT('Ctrl Pts',(9.10058974048747,1.25534320916473,0.605388449123016));
#8965=CARTESIAN_POINT('Ctrl Pts',(8.20058408060299,1.29406305600824,0.605326635812744));
#8966=CARTESIAN_POINT('Ctrl Pts',(7.29999999953093,1.32031613471704,0.605285370449856));
#8967=CARTESIAN_POINT('',(9.99999999523418,1.1090098672342,0.7));
#8968=CARTESIAN_POINT('Ctrl Pts',(9.99999999968202,1.20899340489109,0.605457329065633));
#8969=CARTESIAN_POINT('Ctrl Pts',(9.99999999887489,1.20856043137698,0.613368813757176));
#8970=CARTESIAN_POINT('Ctrl Pts',(9.99999852309337,1.20715974444566,0.621187403383205));
#8971=CARTESIAN_POINT('Ctrl Pts',(9.99999786661901,1.20487567413208,0.628752957409046));
#8972=CARTESIAN_POINT('Ctrl Pts',(9.9999975031266,1.20361097553651,0.63294203403));
#8973=CARTESIAN_POINT('Ctrl Pts',(9.99999733971606,1.20207445367248,0.63705356322819));
#8974=CARTESIAN_POINT('Ctrl Pts',(9.99999742766416,1.20027388348257,0.64105842070465));
#8975=CARTESIAN_POINT('Ctrl Pts',(9.9999975865154,1.19702170610966,0.6482919664668));
#8976=CARTESIAN_POINT('Ctrl Pts',(9.99999868569093,1.19294650045069,0.655099368158521));
#8977=CARTESIAN_POINT('Ctrl Pts',(9.9999991134218,1.18811276085989,0.661317774786376));
#8978=CARTESIAN_POINT('Ctrl Pts',(9.99999919410111,1.18720101282252,0.662490701033652));
#8979=CARTESIAN_POINT('Ctrl Pts',(9.99999924414009,1.18626214680169,0.663642601192937));
#8980=CARTESIAN_POINT('Ctrl Pts',(9.99999924372355,1.18529642131707,0.664772262763739));
#8981=CARTESIAN_POINT('Ctrl Pts',(9.99999924291654,1.18342543943696,0.666960851926287));
#8982=CARTESIAN_POINT('Ctrl Pts',(9.99999905429896,1.18145367213587,0.669066014649603));
#8983=CARTESIAN_POINT('Ctrl Pts',(9.99999879621773,1.17938809187152,0.671084194359814));
#8984=CARTESIAN_POINT('Ctrl Pts',(9.99999808597787,1.17370361260899,0.676638227242868));
#8985=CARTESIAN_POINT('Ctrl Pts',(9.9999969699445,1.16737553754052,0.681473799108647));
#8986=CARTESIAN_POINT('Ctrl Pts',(9.99999660204079,1.16056788011185,0.685537070165577));
#8987=CARTESIAN_POINT('Ctrl Pts',(9.99999636768906,1.15623145667386,0.688125341392612));
#8988=CARTESIAN_POINT('Ctrl Pts',(9.99999638726733,1.15169947441128,0.690399565850749));
#8989=CARTESIAN_POINT('Ctrl Pts',(9.99999666360534,1.14700857532255,0.692336497939236));
#8990=CARTESIAN_POINT('Ctrl Pts',(9.99999709503399,1.13968497812548,0.695360504669253));
#8991=CARTESIAN_POINT('Ctrl Pts',(9.99999815490668,1.13205884654683,0.697530003145419));
#8992=CARTESIAN_POINT('Ctrl Pts',(9.99999900983214,1.12427739544825,0.698775573347137));
#8993=CARTESIAN_POINT('Ctrl Pts',(9.99999956314479,1.11924119569193,0.699581713521624));
#8994=CARTESIAN_POINT('Ctrl Pts',(10.,1.11413933950174,0.7));
#8995=CARTESIAN_POINT('Ctrl Pts',(10.,1.10900986674273,0.7));
#8996=CARTESIAN_POINT('Ctrl Pts',(8.26514054272776,1.18768929227839,0.7));
#8997=CARTESIAN_POINT('Ctrl Pts',(8.84359655063997,1.16547286645366,0.7));
#8998=CARTESIAN_POINT('Ctrl Pts',(9.42188471826001,1.13881853081542,0.7));
#8999=CARTESIAN_POINT('Ctrl Pts',(9.99999999522154,1.10900986698912,0.7));
#9000=CARTESIAN_POINT('Origin',(5.4,-8.11656130105013E-18,0.7));
#9001=CARTESIAN_POINT('',(7.3,-1.22041345053557,0.7));
#9002=CARTESIAN_POINT('Ctrl Pts',(7.94916654049851,-1.19937499624794,0.7));
#9003=CARTESIAN_POINT('Ctrl Pts',(7.73280095382446,-1.20706364505454,0.7));
#9004=CARTESIAN_POINT('Ctrl Pts',(7.51641201888728,-1.21409884616656,0.7));
#9005=CARTESIAN_POINT('Ctrl Pts',(7.29999999989085,-1.22041345054982,0.7));
#9006=CARTESIAN_POINT('',(7.3,-0.712777777777778,0.7));
#9007=CARTESIAN_POINT('',(10.,-1.10900986674244,0.7));
#9008=CARTESIAN_POINT('',(10.,0.653773457742722,0.7));
#9009=CARTESIAN_POINT('Ctrl Pts',(10.,-1.10900986674273,0.7));
#9010=CARTESIAN_POINT('Ctrl Pts',(9.42188472144661,-1.13881853066854,0.7));
#9011=CARTESIAN_POINT('Ctrl Pts',(8.84359655223373,-1.16547286639245,0.7));
#9012=CARTESIAN_POINT('Ctrl Pts',(8.26514054272776,-1.18768929227839,0.7));
#9013=CARTESIAN_POINT('',(7.95,-1.,0.7));
#9014=CARTESIAN_POINT('Origin',(8.1,-1.,0.7));
#9015=CARTESIAN_POINT('',(7.95,1.,0.7));
#9016=CARTESIAN_POINT('Origin',(8.1,1.,0.7));
#9017=CARTESIAN_POINT('',(8.4,-4.89858719658942E-17,0.7));
#9018=CARTESIAN_POINT('Origin',(8.8,0.,0.7));
#9019=CARTESIAN_POINT('Origin',(8.1,-1.,0.8));
#9020=CARTESIAN_POINT('',(7.95,-1.,0.9));
#9021=CARTESIAN_POINT('Origin',(8.1,-1.,0.9));
#9022=CARTESIAN_POINT('',(7.95,-1.,0.8));
#9023=CARTESIAN_POINT('Origin',(2.7,-1.,0.8));
#9024=CARTESIAN_POINT('',(2.55,-1.,0.9));
#9025=CARTESIAN_POINT('Origin',(2.7,-1.,0.9));
#9026=CARTESIAN_POINT('',(2.55,-1.,0.7));
#9027=CARTESIAN_POINT('',(2.55,-1.,0.8));
#9028=CARTESIAN_POINT('Origin',(2.7,-1.,0.7));
#9029=CARTESIAN_POINT('Origin',(2.7,1.,0.8));
#9030=CARTESIAN_POINT('',(2.55,1.,0.9));
#9031=CARTESIAN_POINT('Origin',(2.7,1.,0.9));
#9032=CARTESIAN_POINT('',(2.55,1.,0.7));
#9033=CARTESIAN_POINT('',(2.55,1.,0.8));
#9034=CARTESIAN_POINT('Origin',(2.7,1.,0.7));
#9035=CARTESIAN_POINT('Origin',(8.1,1.,0.8));
#9036=CARTESIAN_POINT('',(7.95,1.,0.9));
#9037=CARTESIAN_POINT('Origin',(8.1,1.,0.9));
#9038=CARTESIAN_POINT('',(7.95,1.,0.8));
#9039=CARTESIAN_POINT('Origin',(2.,0.,0.75));
#9040=CARTESIAN_POINT('',(1.7,3.67394039744206E-17,0.9));
#9041=CARTESIAN_POINT('Origin',(2.,0.,0.9));
#9042=CARTESIAN_POINT('',(1.7,3.67394039744206E-17,0.6));
#9043=CARTESIAN_POINT('',(1.7,3.67394039744206E-17,0.75));
#9044=CARTESIAN_POINT('Origin',(2.,0.,0.6));
#9045=CARTESIAN_POINT('Origin',(2.,0.,0.6));
#9046=CARTESIAN_POINT('',(1.83,-2.0818995585505E-17,0.6));
#9047=CARTESIAN_POINT('Origin',(2.,0.,0.6));
#9048=CARTESIAN_POINT('Origin',(8.8,0.,0.75));
#9049=CARTESIAN_POINT('',(8.5,3.67394039744206E-17,0.9));
#9050=CARTESIAN_POINT('Origin',(8.8,0.,0.9));
#9051=CARTESIAN_POINT('',(8.5,3.67394039744206E-17,0.6));
#9052=CARTESIAN_POINT('',(8.5,3.67394039744206E-17,0.75));
#9053=CARTESIAN_POINT('Origin',(8.8,0.,0.6));
#9054=CARTESIAN_POINT('Origin',(8.8,0.,0.6));
#9055=CARTESIAN_POINT('',(8.63,-2.0818995585505E-17,0.6));
#9056=CARTESIAN_POINT('Origin',(8.8,0.,0.6));
#9057=CARTESIAN_POINT('Origin',(2.,0.,0.45));
#9058=CARTESIAN_POINT('',(1.83,-2.0818995585505E-17,0.32));
#9059=CARTESIAN_POINT('',(1.83,2.0818995585505E-17,0.45));
#9060=CARTESIAN_POINT('Origin',(2.,0.,0.32));
#9061=CARTESIAN_POINT('Origin',(8.8,0.,0.45));
#9062=CARTESIAN_POINT('',(8.63,-2.0818995585505E-17,0.32));
#9063=CARTESIAN_POINT('',(8.63,2.0818995585505E-17,0.45));
#9064=CARTESIAN_POINT('Origin',(8.8,0.,0.32));
#9065=CARTESIAN_POINT('Origin',(10.,-0.62,0.32));
#9066=CARTESIAN_POINT('',(0.200274469199584,-0.62,0.));
#9067=CARTESIAN_POINT('',(0.217044958570157,-0.62,0.32));
#9068=CARTESIAN_POINT('',(0.221783445591644,-0.62,0.410415718550007));
#9069=CARTESIAN_POINT('',(0.,-0.62,0.));
#9070=CARTESIAN_POINT('',(7.7,-0.62,0.));
#9071=CARTESIAN_POINT('',(0.0167704893705732,-0.62,0.32));
#9072=CARTESIAN_POINT('',(0.0220575386407278,-0.62,0.420882909798596));
#9073=CARTESIAN_POINT('',(-0.1,-0.62,0.32));
#9074=CARTESIAN_POINT('Origin',(10.,-0.62,0.32));
#9075=CARTESIAN_POINT('',(0.9,-0.62,0.32));
#9076=CARTESIAN_POINT('',(0.9,-0.62,0.));
#9077=CARTESIAN_POINT('',(0.9,-0.62,0.16));
#9078=CARTESIAN_POINT('',(1.1,-0.62,0.32));
#9079=CARTESIAN_POINT('',(-0.1,-0.62,0.32));
#9080=CARTESIAN_POINT('',(1.1,-0.62,0.));
#9081=CARTESIAN_POINT('',(1.1,-0.62,0.16));
#9082=CARTESIAN_POINT('',(7.7,-0.62,0.));
#9083=CARTESIAN_POINT('Origin',(10.,-0.62,0.32));
#9084=CARTESIAN_POINT('',(3.5,-0.62,0.32));
#9085=CARTESIAN_POINT('',(3.5,-0.62,0.));
#9086=CARTESIAN_POINT('',(3.5,-0.62,0.16));
#9087=CARTESIAN_POINT('',(3.7,-0.62,0.32));
#9088=CARTESIAN_POINT('',(-0.1,-0.62,0.32));
#9089=CARTESIAN_POINT('',(3.7,-0.62,0.));
#9090=CARTESIAN_POINT('',(3.7,-0.62,0.16));
#9091=CARTESIAN_POINT('',(7.7,-0.62,0.));
#9092=CARTESIAN_POINT('Origin',(10.,-0.62,0.32));
#9093=CARTESIAN_POINT('',(7.1,-0.62,0.32));
#9094=CARTESIAN_POINT('',(7.1,-0.62,0.));
#9095=CARTESIAN_POINT('',(7.1,-0.62,0.16));
#9096=CARTESIAN_POINT('',(7.3,-0.62,0.32));
#9097=CARTESIAN_POINT('',(-0.1,-0.62,0.32));
#9098=CARTESIAN_POINT('',(7.3,-0.62,0.));
#9099=CARTESIAN_POINT('',(7.3,-0.62,0.16));
#9100=CARTESIAN_POINT('',(7.7,-0.62,0.));
#9101=CARTESIAN_POINT('Origin',(-0.0999999999999996,0.62,0.32));
#9102=CARTESIAN_POINT('',(0.217044958570158,0.62,0.32));
#9103=CARTESIAN_POINT('',(0.200274469199584,0.62,0.));
#9104=CARTESIAN_POINT('',(0.207951231396534,0.62,0.146481348799182));
#9105=CARTESIAN_POINT('',(0.0167704893705736,0.62,0.32));
#9106=CARTESIAN_POINT('',(10.,0.62,0.32));
#9107=CARTESIAN_POINT('',(0.,0.62,0.));
#9108=CARTESIAN_POINT('',(0.00822532444561912,0.62,0.156948540047771));
#9109=CARTESIAN_POINT('',(2.65,0.62,0.));
#9110=CARTESIAN_POINT('Origin',(-0.0999999999999996,0.62,0.32));
#9111=CARTESIAN_POINT('',(0.9,0.62,0.));
#9112=CARTESIAN_POINT('',(0.9,0.62,0.32));
#9113=CARTESIAN_POINT('',(0.9,0.62,0.16));
#9114=CARTESIAN_POINT('',(1.1,0.62,0.));
#9115=CARTESIAN_POINT('',(2.65,0.62,0.));
#9116=CARTESIAN_POINT('',(1.1,0.62,0.32));
#9117=CARTESIAN_POINT('',(1.1,0.62,0.16));
#9118=CARTESIAN_POINT('',(10.,0.62,0.32));
#9119=CARTESIAN_POINT('Origin',(-0.0999999999999996,0.62,0.32));
#9120=CARTESIAN_POINT('',(3.5,0.62,0.));
#9121=CARTESIAN_POINT('',(3.5,0.62,0.32));
#9122=CARTESIAN_POINT('',(3.5,0.62,0.16));
#9123=CARTESIAN_POINT('',(3.7,0.62,0.));
#9124=CARTESIAN_POINT('',(2.65,0.62,0.));
#9125=CARTESIAN_POINT('',(3.7,0.62,0.32));
#9126=CARTESIAN_POINT('',(3.7,0.62,0.16));
#9127=CARTESIAN_POINT('',(10.,0.62,0.32));
#9128=CARTESIAN_POINT('Origin',(4.95,0.,0.32));
#9129=CARTESIAN_POINT('',(1.6,-4.89858719658941E-17,0.32));
#9130=CARTESIAN_POINT('Origin',(2.,0.,0.32));
#9131=CARTESIAN_POINT('Origin',(4.95,0.,0.32));
#9132=CARTESIAN_POINT('',(8.4,-4.89858719658942E-17,0.32));
#9133=CARTESIAN_POINT('Origin',(8.8,0.,0.32));
#9134=CARTESIAN_POINT('Origin',(4.95,0.,0.32));
#9135=CARTESIAN_POINT('',(0.217044958570157,-0.7,0.32));
#9136=CARTESIAN_POINT('',(0.0167704893705731,-0.7,0.32));
#9137=CARTESIAN_POINT('Origin',(4.95,0.,0.32));
#9138=CARTESIAN_POINT('',(0.9,0.671641708581009,0.32));
#9139=CARTESIAN_POINT('',(1.1,-0.671641708581009,0.32));
#9140=CARTESIAN_POINT('Origin',(4.95,0.,0.32));
#9141=CARTESIAN_POINT('',(3.5,0.723888888888889,0.32));
#9142=CARTESIAN_POINT('',(3.7,-0.723888888888889,0.32));
#9143=CARTESIAN_POINT('Origin',(4.95,0.,0.32));
#9144=CARTESIAN_POINT('',(7.1,0.62,0.32));
#9145=CARTESIAN_POINT('',(7.1,0.712777777777778,0.32));
#9146=CARTESIAN_POINT('',(7.3,0.62,0.32));
#9147=CARTESIAN_POINT('',(10.,0.62,0.32));
#9148=CARTESIAN_POINT('',(7.3,-0.712777777777778,0.32));
#9149=CARTESIAN_POINT('Origin',(-0.0999999999999996,0.62,0.32));
#9150=CARTESIAN_POINT('',(7.1,0.62,0.));
#9151=CARTESIAN_POINT('',(7.1,0.62,0.16));
#9152=CARTESIAN_POINT('',(7.3,0.62,0.));
#9153=CARTESIAN_POINT('',(2.65,0.62,0.));
#9154=CARTESIAN_POINT('',(7.3,0.62,0.16));
#9155=CARTESIAN_POINT('Origin',(10.,1.30754691548544,0.));
#9156=CARTESIAN_POINT('',(10.,1.24211782565704,0.));
#9157=CARTESIAN_POINT('',(10.,-1.24211782565704,0.));
#9158=CARTESIAN_POINT('',(10.,1.30754691548544,0.));
#9159=CARTESIAN_POINT('',(10.,-1.20899340483173,0.605457329065657));
#9160=CARTESIAN_POINT('Ctrl Pts',(10.,-1.20899340483173,0.605457329065657));
#9161=CARTESIAN_POINT('Ctrl Pts',(10.,-1.21451837038612,0.504502771559899));
#9162=CARTESIAN_POINT('Ctrl Pts',(10.,-1.22004249263249,0.403547366186347));
#9163=CARTESIAN_POINT('Ctrl Pts',(10.,-1.23108392958594,0.201728789021226));
#9164=CARTESIAN_POINT('Ctrl Pts',(10.,-1.23660133320922,0.100864020914724));
#9165=CARTESIAN_POINT('Ctrl Pts',(10.,-1.24211782565704,0.));
#9166=CARTESIAN_POINT('Ctrl Pts',(10.,-1.10900986674273,0.7));
#9167=CARTESIAN_POINT('Ctrl Pts',(10.,-1.11692706738765,0.7));
#9168=CARTESIAN_POINT('Ctrl Pts',(9.99999896020971,-1.12478097169818,0.699006158364426));
#9169=CARTESIAN_POINT('Ctrl Pts',(9.99999805494427,-1.13243115645175,0.697118998397561));
#9170=CARTESIAN_POINT('Ctrl Pts',(9.99999754769332,-1.13671781459207,0.696061558623929));
#9171=CARTESIAN_POINT('Ctrl Pts',(9.99999708556116,-1.14094056283945,0.694722610426682));
#9172=CARTESIAN_POINT('Ctrl Pts',(9.99999679002998,-1.14507302265453,0.693112977943955));
#9173=CARTESIAN_POINT('Ctrl Pts',(9.99999625879002,-1.15250143622127,0.690219540062595));
#9174=CARTESIAN_POINT('Ctrl Pts',(9.999996365957,-1.15955821040664,0.686485807665162));
#9175=CARTESIAN_POINT('Ctrl Pts',(9.99999703387985,-1.16609707610076,0.681992895329386));
#9176=CARTESIAN_POINT('Ctrl Pts',(9.99999740034986,-1.16968476316425,0.679527763880215));
#9177=CARTESIAN_POINT('Ctrl Pts',(9.99999792190556,-1.17311627083768,0.676833210412541));
#9178=CARTESIAN_POINT('Ctrl Pts',(9.99999838578331,-1.17636354905877,0.673917165661822));
#9179=CARTESIAN_POINT('Ctrl Pts',(9.99999884023993,-1.17954487655573,0.671060344436104));
#9180=CARTESIAN_POINT('Ctrl Pts',(9.99999924462882,-1.18253006594632,0.668008218820746));
#9181=CARTESIAN_POINT('Ctrl Pts',(9.99999924442301,-1.185296421281,0.664772262763763));
#9182=CARTESIAN_POINT('Ctrl Pts',(9.99999924404215,-1.19041578560695,0.658783864313737));
#9183=CARTESIAN_POINT('Ctrl Pts',(9.99999800949836,-1.19478865237554,0.652167294255586));
#9184=CARTESIAN_POINT('Ctrl Pts',(9.99999759228052,-1.19835462180986,0.645087621913151));
#9185=CARTESIAN_POINT('Ctrl Pts',(9.99999755030119,-1.19871341999785,0.644375284453517));
#9186=CARTESIAN_POINT('Ctrl Pts',(9.9999975145836,-1.19906401030029,0.643658239626438));
#9187=CARTESIAN_POINT('Ctrl Pts',(9.99999748581823,-1.19940630408966,0.642936645100882));
#9188=CARTESIAN_POINT('Ctrl Pts',(9.99999720003888,-1.20280693749908,0.635767720253638));
#9189=CARTESIAN_POINT('Ctrl Pts',(9.9999978299417,-1.20535324884233,0.628234501710241));
#9190=CARTESIAN_POINT('Ctrl Pts',(9.99999874867777,-1.20699142055415,0.62050509267719));
#9191=CARTESIAN_POINT('Ctrl Pts',(9.99999933690345,-1.20804026874419,0.615556297251186));
#9192=CARTESIAN_POINT('Ctrl Pts',(9.99999999916487,-1.20871598809812,0.61052641213707));
#9193=CARTESIAN_POINT('Ctrl Pts',(9.99999999968202,-1.20899340489109,0.605457329065633));
#9194=CARTESIAN_POINT('Ctrl Pts',(10.,1.24211782565704,0.));
#9195=CARTESIAN_POINT('Ctrl Pts',(10.,1.23660053043673,0.100878698875723));
#9196=CARTESIAN_POINT('Ctrl Pts',(10.,1.23108232376984,0.201758145268796));
#9197=CARTESIAN_POINT('Ctrl Pts',(10.,1.22004088630648,0.403576722396156));
#9198=CARTESIAN_POINT('Ctrl Pts',(10.,1.2145175671044,0.504517449470448));
#9199=CARTESIAN_POINT('Ctrl Pts',(10.,1.20899340483173,0.605457329065657));
#9200=CARTESIAN_POINT('Origin',(7.3,-1.42555555555556,0.));
#9201=CARTESIAN_POINT('',(7.3,1.35236351479115,0.));
#9202=CARTESIAN_POINT('',(7.3,-1.42555555555556,0.));
#9203=CARTESIAN_POINT('Ctrl Pts',(7.29999999953133,1.3203161347307,0.605285370449834));
#9204=CARTESIAN_POINT('Ctrl Pts',(7.29999999953133,1.32565322760551,0.504490726585133));
#9205=CARTESIAN_POINT('Ctrl Pts',(7.3,1.33099015509697,0.403695123734478));
#9206=CARTESIAN_POINT('Ctrl Pts',(7.3,1.34167258064689,0.201933969199042));
#9207=CARTESIAN_POINT('Ctrl Pts',(7.3,1.34701817868136,0.100966514951419));
#9208=CARTESIAN_POINT('Ctrl Pts',(7.3,1.35236351479115,0.));
#9209=CARTESIAN_POINT('',(7.29999999953133,-1.3203161347307,0.605285370449834));
#9210=CARTESIAN_POINT('Ctrl Pts',(7.3,-1.32031613470337,0.605285370449877));
#9211=CARTESIAN_POINT('Ctrl Pts',(7.3,-1.31989712778929,0.61319860217968));
#9212=CARTESIAN_POINT('Ctrl Pts',(7.29999916171872,-1.31851071739963,0.621020829077898));
#9213=CARTESIAN_POINT('Ctrl Pts',(7.29999878808195,-1.31624092632926,0.628591660945423));
#9214=CARTESIAN_POINT('Ctrl Pts',(7.29999857947278,-1.31497365483497,0.632818613610392));
#9215=CARTESIAN_POINT('Ctrl Pts',(7.29999848639856,-1.31343001415,0.636967235874856));
#9216=CARTESIAN_POINT('Ctrl Pts',(7.29999853830689,-1.31161789606625,0.641007613679984));
#9217=CARTESIAN_POINT('Ctrl Pts',(7.29999863125487,-1.30837308502546,0.648242386418365));
#9218=CARTESIAN_POINT('Ctrl Pts',(7.29999925734287,-1.30430566789097,0.655052076019481));
#9219=CARTESIAN_POINT('Ctrl Pts',(7.29999949821933,-1.29947941328181,0.661273460789274));
#9220=CARTESIAN_POINT('Ctrl Pts',(7.29999954322,-1.29857776968225,0.662435743389828));
#9221=CARTESIAN_POINT('Ctrl Pts',(7.29999957102613,-1.29764951297213,0.663577423078133));
#9222=CARTESIAN_POINT('Ctrl Pts',(7.2999995707084,-1.29669488998092,0.664697318929248));
#9223=CARTESIAN_POINT('Ctrl Pts',(7.29999957007561,-1.29479368240016,0.666927680549918));
#9224=CARTESIAN_POINT('Ctrl Pts',(7.29999945886743,-1.29278792931167,0.669071688571899));
#9225=CARTESIAN_POINT('Ctrl Pts',(7.29999930790078,-1.2906849717248,0.671125563583336));
#9226=CARTESIAN_POINT('Ctrl Pts',(7.29999889984047,-1.28500071247856,0.676677153447665));
#9227=CARTESIAN_POINT('Ctrl Pts',(7.29999826931494,-1.27867319504519,0.681510485910933));
#9228=CARTESIAN_POINT('Ctrl Pts',(7.29999806345125,-1.27186607945067,0.685571085769401));
#9229=CARTESIAN_POINT('Ctrl Pts',(7.29999793266427,-1.26754145993833,0.688150820039508));
#9230=CARTESIAN_POINT('Ctrl Pts',(7.29999794545359,-1.26302231037287,0.690417984675215));
#9231=CARTESIAN_POINT('Ctrl Pts',(7.29999810371711,-1.25834494218995,0.69234933099425));
#9232=CARTESIAN_POINT('Ctrl Pts',(7.29999835129001,-1.25102809722258,0.695370551698293));
#9233=CARTESIAN_POINT('Ctrl Pts',(7.29999895574222,-1.24340909242398,0.6975375590939));
#9234=CARTESIAN_POINT('Ctrl Pts',(7.29999944081525,-1.2356348173965,0.698780605629559));
#9235=CARTESIAN_POINT('Ctrl Pts',(7.29999975409932,-1.23061380764338,0.699583426311495));
#9236=CARTESIAN_POINT('Ctrl Pts',(7.30000000047446,-1.22552743956586,0.699999999832051));
#9237=CARTESIAN_POINT('Ctrl Pts',(7.29999999989087,-1.22041345054982,0.7));
#9238=CARTESIAN_POINT('',(7.3,-1.35236351479115,0.));
#9239=CARTESIAN_POINT('Ctrl Pts',(7.3,-1.35236351479115,0.));
#9240=CARTESIAN_POINT('Ctrl Pts',(7.3,-1.34701814920095,0.100967071798286));
#9241=CARTESIAN_POINT('Ctrl Pts',(7.3,-1.34167252169398,0.201935082699409));
#9242=CARTESIAN_POINT('Ctrl Pts',(7.3,-1.33099009614589,0.403696237111114));
#9243=CARTESIAN_POINT('Ctrl Pts',(7.29999999953133,-1.32565319812959,0.504491283257837));
#9244=CARTESIAN_POINT('Ctrl Pts',(7.29999999953133,-1.3203161347307,0.605285370449834));
#9245=CARTESIAN_POINT('',(7.3,-1.42555555555556,0.));
#9246=CARTESIAN_POINT('Origin',(3.7,-1.44777777777778,0.));
#9247=CARTESIAN_POINT('',(3.7,1.37924639543935,0.));
#9248=CARTESIAN_POINT('',(3.7,-1.44777777777778,0.));
#9249=CARTESIAN_POINT('',(3.7,1.34735368793805,0.605261457205193));
#9250=CARTESIAN_POINT('Ctrl Pts',(3.7,1.34735368793805,0.605261457205193));
#9251=CARTESIAN_POINT('Ctrl Pts',(3.7,1.35266395147774,0.504488703431434));
#9252=CARTESIAN_POINT('Ctrl Pts',(3.7,1.35797406404029,0.40371594170176));
#9253=CARTESIAN_POINT('Ctrl Pts',(3.7,1.36860496587027,0.201962122597264));
#9254=CARTESIAN_POINT('Ctrl Pts',(3.7,1.37392575452088,0.100981065191366));
#9255=CARTESIAN_POINT('Ctrl Pts',(3.7,1.37924639543935,0.));
#9256=CARTESIAN_POINT('',(3.7,1.24747724070879,0.7));
#9257=CARTESIAN_POINT('Ctrl Pts',(3.7,1.24747724070879,0.7));
#9258=CARTESIAN_POINT('Ctrl Pts',(3.7,1.25538532734776,0.7));
#9259=CARTESIAN_POINT('Ctrl Pts',(3.70000034866643,1.26322972530331,0.699006048248363));
#9260=CARTESIAN_POINT('Ctrl Pts',(3.70000065268588,1.27087026624727,0.697119044026295));
#9261=CARTESIAN_POINT('Ctrl Pts',(3.7000008238479,1.27517186762995,0.696056666371322));
#9262=CARTESIAN_POINT('Ctrl Pts',(3.70000097972585,1.27940891103121,0.694710185093394));
#9263=CARTESIAN_POINT('Ctrl Pts',(3.70000107833511,1.28355469746902,0.693090631030141));
#9264=CARTESIAN_POINT('Ctrl Pts',(3.70000125487464,1.29097687270382,0.690191153635441));
#9265=CARTESIAN_POINT('Ctrl Pts',(3.7000012145424,1.29802606517866,0.686451118058958));
#9266=CARTESIAN_POINT('Ctrl Pts',(3.70000098691147,1.3045562506385,0.681952404110064));
#9267=CARTESIAN_POINT('Ctrl Pts',(3.70000086156653,1.30815209635338,0.679475187900035));
#9268=CARTESIAN_POINT('Ctrl Pts',(3.70000068390876,1.31159030769532,0.676767042898431));
#9269=CARTESIAN_POINT('Ctrl Pts',(3.70000052608992,1.31484259178137,0.673836088143417));
#9270=CARTESIAN_POINT('Ctrl Pts',(3.70000037216713,1.31801458722906,0.670977489418868));
#9271=CARTESIAN_POINT('Ctrl Pts',(3.70000023558528,1.32099045552882,0.667924239810466));
#9272=CARTESIAN_POINT('Ctrl Pts',(3.70000023595245,1.32374763345498,0.664687876924229));
#9273=CARTESIAN_POINT('Ctrl Pts',(3.70000023663259,1.32885491153898,0.658692977181302));
#9274=CARTESIAN_POINT('Ctrl Pts',(3.70000065621025,1.33321474659758,0.652071180203097));
#9275=CARTESIAN_POINT('Ctrl Pts',(3.70000080093706,1.33676785491319,0.644988218508662));
#9276=CARTESIAN_POINT('Ctrl Pts',(3.70000081573428,1.33713113341147,0.644264039153811));
#9277=CARTESIAN_POINT('Ctrl Pts',(3.70000082835625,1.33748593861467,0.643535019157411));
#9278=CARTESIAN_POINT('Ctrl Pts',(3.70000083855542,1.33783217873901,0.642801324492746));
#9279=CARTESIAN_POINT('Ctrl Pts',(3.70000093832019,1.34121897990539,0.63562457699476));
#9280=CARTESIAN_POINT('Ctrl Pts',(3.70000072997693,1.34375116782692,0.628085030530103));
#9281=CARTESIAN_POINT('Ctrl Pts',(3.70000042189378,1.34537558692779,0.6203512574804));
#9282=CARTESIAN_POINT('Ctrl Pts',(3.70000022417294,1.3464181026242,0.615387895628485));
#9283=CARTESIAN_POINT('Ctrl Pts',(3.70000000036652,1.34708586836718,0.6103438638189));
#9284=CARTESIAN_POINT('Ctrl Pts',(3.69999999992214,1.34735368792773,0.6052614572053));
#9285=CARTESIAN_POINT('',(3.7,-1.24747724070944,0.7));
#9286=CARTESIAN_POINT('',(3.7,-0.723888888888889,0.7));
#9287=CARTESIAN_POINT('',(3.7,-1.34735368793805,0.605261457205193));
#9288=CARTESIAN_POINT('Ctrl Pts',(3.69999999992215,-1.34735368792773,0.6052614572053));
#9289=CARTESIAN_POINT('Ctrl Pts',(3.70000000061408,-1.34693666923469,0.613175212866596));
#9290=CARTESIAN_POINT('Ctrl Pts',(3.70000049671034,-1.34555248374866,0.620998392122869));
#9291=CARTESIAN_POINT('Ctrl Pts',(3.70000071566022,-1.34328499565267,0.628570462735333));
#9292=CARTESIAN_POINT('Ctrl Pts',(3.70000083807517,-1.34201724238155,0.632804009674372));
#9293=CARTESIAN_POINT('Ctrl Pts',(3.7000008913247,-1.34047237297042,0.63695909738719));
#9294=CARTESIAN_POINT('Ctrl Pts',(3.70000085837557,-1.33865827982058,0.641005656934072));
#9295=CARTESIAN_POINT('Ctrl Pts',(3.7000007994669,-1.33541492172585,0.648240369034365));
#9296=CARTESIAN_POINT('Ctrl Pts',(3.70000042420685,-1.33134915897915,0.655050234746405));
#9297=CARTESIAN_POINT('Ctrl Pts',(3.70000027984635,-1.32652447879733,0.661271863919233));
#9298=CARTESIAN_POINT('Ctrl Pts',(3.70000025294096,-1.32562527203035,0.662431429080655));
#9299=CARTESIAN_POINT('Ctrl Pts',(3.7000002362737,-1.32469957579387,0.663570491348455));
#9300=CARTESIAN_POINT('Ctrl Pts',(3.70000023630138,-1.32374763346102,0.664687876924223));
#9301=CARTESIAN_POINT('Ctrl Pts',(3.70000023635686,-1.32184039796576,0.666926581264246));
#9302=CARTESIAN_POINT('Ctrl Pts',(3.70000030283857,-1.31982784222224,0.669078323867587));
#9303=CARTESIAN_POINT('Ctrl Pts',(3.70000039320883,-1.31771738411303,0.671139279696989));
#9304=CARTESIAN_POINT('Ctrl Pts',(3.70000063660146,-1.3120333248939,0.676690015307994));
#9305=CARTESIAN_POINT('Ctrl Pts',(3.7000010126336,-1.30570602994251,0.681522474044465));
#9306=CARTESIAN_POINT('Ctrl Pts',(3.70000113724274,-1.29889910811053,0.685582059356066));
#9307=CARTESIAN_POINT('Ctrl Pts',(3.70000121634872,-1.29457784995583,0.688159217808216));
#9308=CARTESIAN_POINT('Ctrl Pts',(3.70000121058612,-1.2900623422215,0.690424215862126));
#9309=CARTESIAN_POINT('Ctrl Pts',(3.70000111831253,-1.28538881676413,0.692353818784707));
#9310=CARTESIAN_POINT('Ctrl Pts',(3.70000097388434,-1.27807373536961,0.695374066040565));
#9311=CARTESIAN_POINT('Ctrl Pts',(3.70000061691996,-1.27045659963863,0.697540160564298));
#9312=CARTESIAN_POINT('Ctrl Pts',(3.7000003304055,-1.26268427129293,0.698782316368755));
#9313=CARTESIAN_POINT('Ctrl Pts',(3.70000014548661,-1.25766794365683,0.699584014420239));
#9314=CARTESIAN_POINT('Ctrl Pts',(3.7,-1.25258637988459,0.7));
#9315=CARTESIAN_POINT('Ctrl Pts',(3.7,-1.24747724070879,0.7));
#9316=CARTESIAN_POINT('',(3.7,-1.37924639543935,0.));
#9317=CARTESIAN_POINT('Ctrl Pts',(3.7,-1.37924639543935,0.));
#9318=CARTESIAN_POINT('Ctrl Pts',(3.7,-1.37392574223662,0.100981298335747));
#9319=CARTESIAN_POINT('Ctrl Pts',(3.7,-1.36860494130098,0.201962588887634));
#9320=CARTESIAN_POINT('Ctrl Pts',(3.7,-1.35797403946962,0.403716407992068));
#9321=CARTESIAN_POINT('Ctrl Pts',(3.7,-1.3526639391921,0.504488936575732));
#9322=CARTESIAN_POINT('Ctrl Pts',(3.7,-1.34735368793805,0.605261457205193));
#9323=CARTESIAN_POINT('',(3.7,-1.44777777777778,0.));
#9324=CARTESIAN_POINT('Origin',(1.1,-1.34328341716202,0.));
#9325=CARTESIAN_POINT('',(1.1,1.27885335043294,0.));
#9326=CARTESIAN_POINT('',(1.1,-1.34328341716202,0.));
#9327=CARTESIAN_POINT('Ctrl Pts',(1.1,1.24553911298206,0.605485603995113));
#9328=CARTESIAN_POINT('Ctrl Pts',(1.1,1.25109559382646,0.504544105903265));
#9329=CARTESIAN_POINT('Ctrl Pts',(1.1,1.25665083308595,0.403601248768354));
#9330=CARTESIAN_POINT('Ctrl Pts',(1.1,1.26775551906787,0.201773573764085));
#9331=CARTESIAN_POINT('Ctrl Pts',(1.1,1.2733051088238,0.100886182270816));
#9332=CARTESIAN_POINT('Ctrl Pts',(1.1,1.27885335043294,0.));
#9333=CARTESIAN_POINT('',(1.1,-1.14549341399195,0.7));
#9334=CARTESIAN_POINT('',(1.1,-0.671641708581009,0.7));
#9335=CARTESIAN_POINT('',(1.1,-1.24553911298206,0.605485603995113));
#9336=CARTESIAN_POINT('Ctrl Pts',(1.09999999916631,-1.24553911263843,0.605485603997431));
#9337=CARTESIAN_POINT('Ctrl Pts',(1.10000000220634,-1.24510362317222,0.61339691285734));
#9338=CARTESIAN_POINT('Ctrl Pts',(1.10000177015643,-1.24370036622144,0.621215229994996));
#9339=CARTESIAN_POINT('Ctrl Pts',(1.10000252895322,-1.24141353486351,0.628780213666851));
#9340=CARTESIAN_POINT('Ctrl Pts',(1.10000294802756,-1.24015054543059,0.632958263090869));
#9341=CARTESIAN_POINT('Ctrl Pts',(1.10000312162076,-1.23861706177488,0.637059070655947));
#9342=CARTESIAN_POINT('Ctrl Pts',(1.10000299297862,-1.23682078380192,0.641053713130525));
#9343=CARTESIAN_POINT('Ctrl Pts',(1.10000275999609,-1.23356756237267,0.64828837095969));
#9344=CARTESIAN_POINT('Ctrl Pts',(1.10000138715103,-1.22949085733774,0.655096441442141));
#9345=CARTESIAN_POINT('Ctrl Pts',(1.10000084482056,-1.2246552743941,0.661315040399663));
#9346=CARTESIAN_POINT('Ctrl Pts',(1.10000074196669,-1.22373819809959,0.662494407966206));
#9347=CARTESIAN_POINT('Ctrl Pts',(1.1000006773267,-1.22279369438101,0.663652502541609));
#9348=CARTESIAN_POINT('Ctrl Pts',(1.10000067553493,-1.22182202641035,0.66478809188211));
#9349=CARTESIAN_POINT('Ctrl Pts',(1.10000067210542,-1.219962222636,0.666961646435043));
#9350=CARTESIAN_POINT('Ctrl Pts',(1.10000089707048,-1.21800293160495,0.669052796220007));
#9351=CARTESIAN_POINT('Ctrl Pts',(1.10000120920309,-1.21595100691259,0.671058078730413));
#9352=CARTESIAN_POINT('Ctrl Pts',(1.10000207391986,-1.21026645613745,0.676613414309409));
#9353=CARTESIAN_POINT('Ctrl Pts',(1.1000034579227,-1.20393786500476,0.681450029097565));
#9354=CARTESIAN_POINT('Ctrl Pts',(1.10000394126019,-1.19712964857754,0.685514663758263));
#9355=CARTESIAN_POINT('Ctrl Pts',(1.10000424974863,-1.19278432848208,0.688108902478585));
#9356=CARTESIAN_POINT('Ctrl Pts',(1.10000425197701,-1.18824265871575,0.690387991283085));
#9357=CARTESIAN_POINT('Ctrl Pts',(1.10000394032285,-1.18354156621637,0.692328715646671));
#9358=CARTESIAN_POINT('Ctrl Pts',(1.10000345443802,-1.17621232165581,0.695354404566264));
#9359=CARTESIAN_POINT('Ctrl Pts',(1.10000219938511,-1.16858027633095,0.697525330589554));
#9360=CARTESIAN_POINT('Ctrl Pts',(1.10000118192936,-1.16079305972554,0.698772417158578));
#9361=CARTESIAN_POINT('Ctrl Pts',(1.10000052251962,-1.15574619011492,0.699580649884844));
#9362=CARTESIAN_POINT('Ctrl Pts',(1.1,-1.15063354328712,0.7));
#9363=CARTESIAN_POINT('Ctrl Pts',(1.1,-1.14549341399196,0.7));
#9364=CARTESIAN_POINT('',(1.1,-1.27885335043294,0.));
#9365=CARTESIAN_POINT('Ctrl Pts',(1.1,-1.27885335043294,0.));
#9366=CARTESIAN_POINT('Ctrl Pts',(1.1,-1.27330503870861,0.100887457206881));
#9367=CARTESIAN_POINT('Ctrl Pts',(1.1,-1.26775537880223,0.201776123688554));
#9368=CARTESIAN_POINT('Ctrl Pts',(1.1,-1.25665069275548,0.403603798678134));
#9369=CARTESIAN_POINT('Ctrl Pts',(1.1,-1.25109552364596,0.504545380833391));
#9370=CARTESIAN_POINT('Ctrl Pts',(1.1,-1.24553911298206,0.605485603995113));
#9371=CARTESIAN_POINT('',(1.1,-1.34328341716202,0.));
#9372=CARTESIAN_POINT('Origin',(0.199725906950915,-1.4,-0.0104671912485888));
#9373=CARTESIAN_POINT('',(0.200274469199584,1.12301388185427,1.38777878078145E-17));
#9374=CARTESIAN_POINT('',(0.200274469199585,-0.7,0.));
#9375=CARTESIAN_POINT('',(0.231993417893744,1.09142177001972,0.605233595624295));
#9376=CARTESIAN_POINT('Ctrl Pts',(0.200274469199584,1.12301388185427,-2.97071395261028E-17));
#9377=CARTESIAN_POINT('Ctrl Pts',(0.210847451470635,1.11248294808,0.201744519910852));
#9378=CARTESIAN_POINT('Ctrl Pts',(0.22142043436526,1.101952242875,0.403489051720196));
#9379=CARTESIAN_POINT('Ctrl Pts',(0.231993417893744,1.09142177001972,0.605233595624295));
#9380=CARTESIAN_POINT('',(0.231993417893744,-1.09142177001972,0.605233595624295));
#9381=CARTESIAN_POINT('',(0.231993417893744,-0.7,0.605233595624295));
#9382=CARTESIAN_POINT('',(0.200274469199584,-1.12301388185427,-1.38777878078145E-17));
#9383=CARTESIAN_POINT('Ctrl Pts',(0.231993417893744,-1.09142177001972,0.605233595624295));
#9384=CARTESIAN_POINT('Ctrl Pts',(0.22142043436526,-1.101952242875,0.403489051720196));
#9385=CARTESIAN_POINT('Ctrl Pts',(0.210847451470635,-1.11248294808,0.201744519910852));
#9386=CARTESIAN_POINT('Ctrl Pts',(0.200274469199584,-1.12301388185427,-4.90059381963448E-17));
#9387=CARTESIAN_POINT('',(0.200274469199585,-0.7,0.));
#9388=CARTESIAN_POINT('Origin',(5.4,-1.11022302462516E-16,0.));
#9389=CARTESIAN_POINT('Ctrl Pts',(7.29999999999999,-1.35236351479115,1.04083408558608E-17));
#9390=CARTESIAN_POINT('Ctrl Pts',(8.20044803681595,-1.32637404707459,3.18306896032855E-8));
#9391=CARTESIAN_POINT('Ctrl Pts',(9.10060048441536,-1.28803709316692,1.03188250195688E-8));
#9392=CARTESIAN_POINT('Ctrl Pts',(10.0000000000405,-1.24211782537639,-8.23328475353175E-12));
#9393=CARTESIAN_POINT('Ctrl Pts',(10.0000000000405,1.24211782537639,-8.23320567538283E-12));
#9394=CARTESIAN_POINT('Ctrl Pts',(9.1006004808701,1.28803709334794,1.03184817085883E-8));
#9395=CARTESIAN_POINT('Ctrl Pts',(8.20044803144508,1.32637404722969,3.18291413954212E-8));
#9396=CARTESIAN_POINT('Ctrl Pts',(7.3,1.35236351479115,4.75121773919879E-17));
#9397=CARTESIAN_POINT('',(7.1,1.35793097395724,0.));
#9398=CARTESIAN_POINT('',(7.1,1.42555555555556,0.));
#9399=CARTESIAN_POINT('Ctrl Pts',(7.1000000000396,1.35793097389613,-4.88924676637329E-12));
#9400=CARTESIAN_POINT('Ctrl Pts',(6.53177385320612,1.37316067096195,3.71763852401782E-9));
#9401=CARTESIAN_POINT('Ctrl Pts',(5.96344379069665,1.38333257666104,-3.82408184804385E-8));
#9402=CARTESIAN_POINT('Ctrl Pts',(5.39512359652123,1.38725406840392,-3.97623797275691E-8));
#9403=CARTESIAN_POINT('Ctrl Pts',(4.82973248928002,1.39115534902226,-4.12760989429076E-8));
#9404=CARTESIAN_POINT('Ctrl Pts',(4.26470859812609,1.38886839226708,1.63957607983357E-8));
#9405=CARTESIAN_POINT('Ctrl Pts',(3.70000000036239,1.37924639538501,-6.25376529969227E-12));
#9406=CARTESIAN_POINT('',(3.5,1.37552980833516,0.));
#9407=CARTESIAN_POINT('',(3.5,1.44777777777778,0.));
#9408=CARTESIAN_POINT('Ctrl Pts',(3.50000000097466,1.37552980835479,1.06251812903579E-15));
#9409=CARTESIAN_POINT('Ctrl Pts',(2.69943075695685,1.35940904975719,2.35366119539541E-7));
#9410=CARTESIAN_POINT('Ctrl Pts',(1.89948254587541,1.32827224396921,2.51300192353997E-7));
#9411=CARTESIAN_POINT('Ctrl Pts',(1.10000000028363,1.27885335028943,-5.13283415455519E-11));
#9412=CARTESIAN_POINT('',(0.9,1.266106713614,0.));
#9413=CARTESIAN_POINT('',(0.9,1.34328341716202,0.));
#9414=CARTESIAN_POINT('',(0.292382661757373,1.22257596919059,0.));
#9415=CARTESIAN_POINT('Ctrl Pts',(0.9,1.266106713614,1.20346441145891E-16));
#9416=CARTESIAN_POINT('Ctrl Pts',(0.697432754539207,1.25280566772398,-2.10387859372414E-8));
#9417=CARTESIAN_POINT('Ctrl Pts',(0.494894520889663,1.23831317328004,3.6654767345328E-12));
#9418=CARTESIAN_POINT('Ctrl Pts',(0.292382661757371,1.22257596919059,2.98331735103528E-16));
#9419=CARTESIAN_POINT('Ctrl Pts',(0.292382661757373,1.22257596919059,2.94902990916057E-17));
#9420=CARTESIAN_POINT('Ctrl Pts',(0.284469747869226,1.22196105627757,-8.65621238729993E-13));
#9421=CARTESIAN_POINT('Ctrl Pts',(0.276673396002317,1.22038240716686,-1.19564355630166E-6));
#9422=CARTESIAN_POINT('Ctrl Pts',(0.269153172408756,1.21792571627104,-1.29137975931779E-6));
#9423=CARTESIAN_POINT('Ctrl Pts',(0.264330998492885,1.21635041859408,-1.35276844214688E-6));
#9424=CARTESIAN_POINT('Ctrl Pts',(0.259622238853914,1.21441292414196,-1.0165784587106E-6));
#9425=CARTESIAN_POINT('Ctrl Pts',(0.255072584042237,1.21212521597766,-4.21167369976509E-7));
#9426=CARTESIAN_POINT('Ctrl Pts',(0.247984787860257,1.20856125126747,5.06409032217246E-7));
#9427=CARTESIAN_POINT('Ctrl Pts',(0.241364979299678,1.20419126978451,2.25366520907849E-6));
#9428=CARTESIAN_POINT('Ctrl Pts',(0.235375785094684,1.19908071490398,1.28723124315333E-6));
#9429=CARTESIAN_POINT('Ctrl Pts',(0.235058634311792,1.19881009144014,1.23605486142058E-6));
#9430=CARTESIAN_POINT('Ctrl Pts',(0.234743258170683,1.19853738091759,1.17639378419006E-6));
#9431=CARTESIAN_POINT('Ctrl Pts',(0.234429683218046,1.19826258967301,1.10742116603597E-6));
#9432=CARTESIAN_POINT('Ctrl Pts',(0.23095881299434,1.19522100506769,3.4398325561458E-7));
#9433=CARTESIAN_POINT('Ctrl Pts',(0.227708211416394,1.19192479473749,-1.52348441667556E-6));
#9434=CARTESIAN_POINT('Ctrl Pts',(0.224692430858345,1.18840300965977,-3.42436181452249E-6));
#9435=CARTESIAN_POINT('Ctrl Pts',(0.219522873151367,1.18236607466387,-6.68278702580898E-6));
#9436=CARTESIAN_POINT('Ctrl Pts',(0.21509942609515,1.17573654654733,-9.78259773483875E-6));
#9437=CARTESIAN_POINT('Ctrl Pts',(0.211478909386775,1.16867548752938,-1.04320859863301E-5));
#9438=CARTESIAN_POINT('Ctrl Pts',(0.20968494559888,1.16517673715679,-1.075390701291E-5));
#9439=CARTESIAN_POINT('Ctrl Pts',(0.208088728862602,1.16157146972622,-1.05358292927083E-5));
#9440=CARTESIAN_POINT('Ctrl Pts',(0.206701335101202,1.15787708229469,-9.83193564179307E-6));
#9441=CARTESIAN_POINT('Ctrl Pts',(0.203919119965097,1.15046852899383,-8.42037994342582E-6));
#9442=CARTESIAN_POINT('Ctrl Pts',(0.202003457218558,1.1427818296106,-4.88542801801716E-6));
#9443=CARTESIAN_POINT('Ctrl Pts',(0.201024541128784,1.13496408391561,-2.30807221316776E-6));
#9444=CARTESIAN_POINT('Ctrl Pts',(0.200529226009753,1.13100843574523,-1.00397341389412E-6));
#9445=CARTESIAN_POINT('Ctrl Pts',(0.200274469344113,1.12701892049093,-1.14168925800036E-11));
#9446=CARTESIAN_POINT('Ctrl Pts',(0.200274469199584,1.12301388185427,-1.43114686768087E-17));
#9447=CARTESIAN_POINT('',(-1.73234772679968E-18,1.12356026268968,4.53319947845445E-20));
#9448=CARTESIAN_POINT('',(0.,-1.4,0.));
#9449=CARTESIAN_POINT('',(0.276326924564679,1.42224670711126,-2.77555756156289E-17));
#9450=CARTESIAN_POINT('Ctrl Pts',(0.276326924564681,1.42224670711126,-1.50920942409982E-16));
#9451=CARTESIAN_POINT('Ctrl Pts',(0.258529852003869,1.4208638358667,-3.32972379743633E-13));
#9452=CARTESIAN_POINT('Ctrl Pts',(0.240927013527826,1.41785398988725,-1.99727536601662E-6));
#9453=CARTESIAN_POINT('Ctrl Pts',(0.223720619657732,1.41333325652174,-2.71091968639774E-6));
#9454=CARTESIAN_POINT('Ctrl Pts',(0.206313289378911,1.40875972999491,-3.432897951005E-6));
#9455=CARTESIAN_POINT('Ctrl Pts',(0.18931019325249,1.40263932318529,-2.78724979559428E-6));
#9456=CARTESIAN_POINT('Ctrl Pts',(0.172932985028856,1.39504220432096,-6.31841720307455E-7));
#9457=CARTESIAN_POINT('Ctrl Pts',(0.170060146426803,1.39370954151055,-2.53746782677961E-7));
#9458=CARTESIAN_POINT('Ctrl Pts',(0.167206630967902,1.39233132643846,1.61597591574489E-7));
#9459=CARTESIAN_POINT('Ctrl Pts',(0.164373729059928,1.39090779908693,6.02790108062464E-7));
#9460=CARTESIAN_POINT('Ctrl Pts',(0.148213121449433,1.38278712717586,3.11962244863226E-6));
#9461=CARTESIAN_POINT('Ctrl Pts',(0.132864864406694,1.37326763401578,6.8005293729143E-6));
#9462=CARTESIAN_POINT('Ctrl Pts',(0.118540368157823,1.36244192017091,7.47011412280372E-6));
#9463=CARTESIAN_POINT('Ctrl Pts',(0.1130124780146,1.35826422653222,7.72851001154276E-6));
#9464=CARTESIAN_POINT('Ctrl Pts',(0.107637267132642,1.35389150739715,7.50091387420595E-6));
#9465=CARTESIAN_POINT('Ctrl Pts',(0.102427993107927,1.34932731552598,6.39696583889361E-6));
#9466=CARTESIAN_POINT('Ctrl Pts',(0.0920147884934566,1.34020361352282,4.19020214765608E-6));
#9467=CARTESIAN_POINT('Ctrl Pts',(0.082263696775192,1.33031540618347,-1.43705507633734E-6));
#9468=CARTESIAN_POINT('Ctrl Pts',(0.0732179607829324,1.31975004019149,-7.24116446069057E-6));
#9469=CARTESIAN_POINT('Ctrl Pts',(0.0614369648181435,1.30598990677343,-1.48003270644599E-5));
#9470=CARTESIAN_POINT('Ctrl Pts',(0.0509520748529884,1.29120077200215,-2.24515165560165E-5));
#9471=CARTESIAN_POINT('Ctrl Pts',(0.0418305631051555,1.27560026299671,-2.64881615939377E-5));
#9472=CARTESIAN_POINT('Ctrl Pts',(0.0329966685655992,1.26049166530727,-3.03975241584371E-5));
#9473=CARTESIAN_POINT('Ctrl Pts',(0.0254411283904758,1.24462062939249,-3.09701348507133E-5));
#9474=CARTESIAN_POINT('Ctrl Pts',(0.0192647836588538,1.2281607987719,-2.81763116144976E-5));
#9475=CARTESIAN_POINT('Ctrl Pts',(0.0129258683931997,1.2112677210496,-2.53089508159798E-5));
#9476=CARTESIAN_POINT('Ctrl Pts',(0.00809110271874438,1.19389182855556,
-1.89493195503086E-5));
#9477=CARTESIAN_POINT('Ctrl Pts',(0.00484442764459327,1.17622983835018,
-1.25518552566888E-5));
#9478=CARTESIAN_POINT('Ctrl Pts',(0.00165723550742335,1.1588914367474,-6.27160009448058E-6));
#9479=CARTESIAN_POINT('Ctrl Pts',(1.90718451428807E-9,1.14127598190669,
-1.51296892603399E-10));
#9480=CARTESIAN_POINT('Ctrl Pts',(2.41777084464267E-17,1.12356026268968,
-3.46944695195361E-18));
#9481=CARTESIAN_POINT('',(10.5166159648474,1.4155315881283,0.));
#9482=CARTESIAN_POINT('Ctrl Pts',(0.276326924564679,1.42224670711126,0.));
#9483=CARTESIAN_POINT('Ctrl Pts',(3.68975660465893,1.68747752195839,0.));
#9484=CARTESIAN_POINT('Ctrl Pts',(7.10318628475318,1.599994843061,0.));
#9485=CARTESIAN_POINT('Ctrl Pts',(10.5166159648474,1.4155315881283,0.));
#9486=CARTESIAN_POINT('',(10.8,1.11638029377732,-5.56631991785941E-17));
#9487=CARTESIAN_POINT('Ctrl Pts',(10.8,1.11638029377732,2.32452945780892E-16));
#9488=CARTESIAN_POINT('Ctrl Pts',(10.7999999994302,1.13421844616111,-9.29296349749781E-12));
#9489=CARTESIAN_POINT('Ctrl Pts',(10.7983603663884,1.15198349698667,-2.38856955364628E-6));
#9490=CARTESIAN_POINT('Ctrl Pts',(10.7951843826221,1.16946861094468,-3.77014304120448E-6));
#9491=CARTESIAN_POINT('Ctrl Pts',(10.7919669771209,1.18718176881198,-5.16973525142236E-6));
#9492=CARTESIAN_POINT('Ctrl Pts',(10.7871724978816,1.20460918321158,-5.4755482503851E-6));
#9493=CARTESIAN_POINT('Ctrl Pts',(10.7808573412527,1.22152732075962,-4.27334038376583E-6));
#9494=CARTESIAN_POINT('Ctrl Pts',(10.7797421066656,1.22451500471617,-4.06103467663179E-6));
#9495=CARTESIAN_POINT('Ctrl Pts',(10.7785793293545,1.22748675045939,-3.81081650224554E-6));
#9496=CARTESIAN_POINT('Ctrl Pts',(10.7773691713543,1.23044124224994,-3.53261416912234E-6));
#9497=CARTESIAN_POINT('Ctrl Pts',(10.7705159051166,1.24717287467681,-1.95712183132163E-6));
#9498=CARTESIAN_POINT('Ctrl Pts',(10.7622076549587,1.26320448426569,8.50150473021234E-7));
#9499=CARTESIAN_POINT('Ctrl Pts',(10.7525236566209,1.27832128496499,1.09915986206012E-6));
#9500=CARTESIAN_POINT('Ctrl Pts',(10.7482509716548,1.28499098118248,1.20902550183604E-6));
#9501=CARTESIAN_POINT('Ctrl Pts',(10.7437098328292,1.29148238441373,7.76315258636623E-7));
#9502=CARTESIAN_POINT('Ctrl Pts',(10.7389041877712,1.29777551763099,-7.54184826032082E-7));
#9503=CARTESIAN_POINT('Ctrl Pts',(10.7310976851069,1.30799836193882,-3.24039694621926E-6));
#9504=CARTESIAN_POINT('Ctrl Pts',(10.7225935645301,1.31769858917671,-8.57388820182801E-6));
#9505=CARTESIAN_POINT('Ctrl Pts',(10.7134588931078,1.3268364513864,-1.41086939541967E-5));
#9506=CARTESIAN_POINT('Ctrl Pts',(10.7004433550849,1.33985653580309,-2.19949628070403E-5));
#9507=CARTESIAN_POINT('Ctrl Pts',(10.6862650266646,1.35162127070648,-3.0022236679635E-5));
#9508=CARTESIAN_POINT('Ctrl Pts',(10.6711476119081,1.36204513612776,-3.40981369893719E-5));
#9509=CARTESIAN_POINT('Ctrl Pts',(10.6560301971515,1.37246900154903,-3.81740372991087E-5));
#9510=CARTESIAN_POINT('Ctrl Pts',(10.6399721826852,1.38155285075117,-3.83332859284948E-5));
#9511=CARTESIAN_POINT('Ctrl Pts',(10.6231652498763,1.38916602817047,-3.45204725343976E-5));
#9512=CARTESIAN_POINT('Ctrl Pts',(10.6063487480974,1.39678354012646,-3.07054883279539E-5));
#9513=CARTESIAN_POINT('Ctrl Pts',(10.5889271210941,1.40286310406803,-2.29928881382306E-5));
#9514=CARTESIAN_POINT('Ctrl Pts',(10.5711041279812,1.40730078588308,-1.53078138731408E-5));
#9515=CARTESIAN_POINT('Ctrl Pts',(10.5532811348684,1.41173846769814,-7.6227396080509E-6));
#9516=CARTESIAN_POINT('Ctrl Pts',(10.5350552605908,1.41453511891929,-9.16729947674095E-11));
#9517=CARTESIAN_POINT('Ctrl Pts',(10.5166159648474,1.4155315881283,2.48932818802672E-16));
#9518=CARTESIAN_POINT('',(10.8,-1.11638029377732,-1.39157997946485E-17));
#9519=CARTESIAN_POINT('',(10.8,1.4,0.));
#9520=CARTESIAN_POINT('',(10.5166159648474,-1.4155315881283,2.77555756156289E-17));
#9521=CARTESIAN_POINT('Ctrl Pts',(10.5166159648474,-1.4155315881283,-1.94289029309402E-16));
#9522=CARTESIAN_POINT('Ctrl Pts',(10.5344251606169,-1.41456917089032,1.72780596414851E-12));
#9523=CARTESIAN_POINT('Ctrl Pts',(10.5520727686739,-1.41197333457428,-2.53403886306205E-6));
#9524=CARTESIAN_POINT('Ctrl Pts',(10.5693578805681,-1.40785843881911,-4.04156906196095E-6));
#9525=CARTESIAN_POINT('Ctrl Pts',(10.5868701251756,-1.40368947182374,-5.56890876087065E-6));
#9526=CARTESIAN_POINT('Ctrl Pts',(10.604011804524,-1.39796079212135,-5.98742339745246E-6));
#9527=CARTESIAN_POINT('Ctrl Pts',(10.6205627760847,-1.39074087128671,-4.81856832951796E-6));
#9528=CARTESIAN_POINT('Ctrl Pts',(10.6234754753687,-1.38947028374636,-4.61286902618664E-6));
#9529=CARTESIAN_POINT('Ctrl Pts',(10.6263698187278,-1.38815339768352,-4.36721670635639E-6));
#9530=CARTESIAN_POINT('Ctrl Pts',(10.629244514885,-1.38679044403738,-4.09122931699412E-6));
#9531=CARTESIAN_POINT('Ctrl Pts',(10.6455827855986,-1.37904412775797,-2.5226612199239E-6));
#9532=CARTESIAN_POINT('Ctrl Pts',(10.6611432679573,-1.36988219838444,3.58605122725343E-7));
#9533=CARTESIAN_POINT('Ctrl Pts',(10.6757157985124,-1.35939560704671,7.40589063327193E-7));
#9534=CARTESIAN_POINT('Ctrl Pts',(10.6821516119741,-1.35476430808026,9.09288478831296E-7));
#9535=CARTESIAN_POINT('Ctrl Pts',(10.6883944859408,-1.34987400891586,5.44816430868337E-7));
#9536=CARTESIAN_POINT('Ctrl Pts',(10.6944246343503,-1.34472976213865,-9.14752338109426E-7));
#9537=CARTESIAN_POINT('Ctrl Pts',(10.7041966733629,-1.33639335368171,-3.28002794718031E-6));
#9538=CARTESIAN_POINT('Ctrl Pts',(10.7134106653983,-1.3273903805878,-8.47259327327479E-6));
#9539=CARTESIAN_POINT('Ctrl Pts',(10.7220307555455,-1.31778973409553,-1.38734771921913E-5));
#9540=CARTESIAN_POINT('Ctrl Pts',(10.7343338492722,-1.3040871333553,-2.15819326638919E-5));
#9541=CARTESIAN_POINT('Ctrl Pts',(10.7453199276401,-1.28929041974124,-2.94555326738194E-5));
#9542=CARTESIAN_POINT('Ctrl Pts',(10.7549158277293,-1.27362793268665,-3.3443536645081E-5));
#9543=CARTESIAN_POINT('Ctrl Pts',(10.7645117278185,-1.25796544563206,-3.74315406163426E-5));
#9544=CARTESIAN_POINT('Ctrl Pts',(10.7727182208071,-1.24143562566754,-3.75750290962259E-5));
#9545=CARTESIAN_POINT('Ctrl Pts',(10.7794153247677,-1.22423716044977,-3.38265125308188E-5));
#9546=CARTESIAN_POINT('Ctrl Pts',(10.7861166764432,-1.20702778690835,-3.00756184258222E-5));
#9547=CARTESIAN_POINT('Ctrl Pts',(10.7912490477072,-1.18929683429644,-2.25107044755726E-5));
#9548=CARTESIAN_POINT('Ctrl Pts',(10.7947196858669,-1.17125359626911,-1.49815203503087E-5));
#9549=CARTESIAN_POINT('Ctrl Pts',(10.7981903240266,-1.15321035824179,-7.45233622504479E-6));
#9550=CARTESIAN_POINT('Ctrl Pts',(10.7999999985278,-1.13485327409571,-1.17780195603766E-10));
#9551=CARTESIAN_POINT('Ctrl Pts',(10.8,-1.11638029377732,-1.38777878078145E-17));
#9552=CARTESIAN_POINT('',(0.276326924564679,-1.42224670711126,-5.55111512312578E-17));
#9553=CARTESIAN_POINT('Ctrl Pts',(10.5166159648474,-1.4155315881283,0.));
#9554=CARTESIAN_POINT('Ctrl Pts',(7.10318628475318,-1.599994843061,0.));
#9555=CARTESIAN_POINT('Ctrl Pts',(3.68975660465893,-1.68747752195839,0.));
#9556=CARTESIAN_POINT('Ctrl Pts',(0.276326924564679,-1.42224670711126,0.));
#9557=CARTESIAN_POINT('',(-7.25311916552711E-19,-1.12356026268968,1.39157997946485E-17));
#9558=CARTESIAN_POINT('Ctrl Pts',(1.80411241501588E-16,-1.12356026268968,
-1.53523027623947E-16));
#9559=CARTESIAN_POINT('Ctrl Pts',(7.41078168374529E-10,-1.14141522098415,
-1.3067981184062E-11));
#9560=CARTESIAN_POINT('Ctrl Pts',(0.00163694718329378,-1.15920272117896,
-1.78823819589733E-6));
#9561=CARTESIAN_POINT('Ctrl Pts',(0.00481087395297265,-1.17671209893291,
-2.3181425555783E-6));
#9562=CARTESIAN_POINT('Ctrl Pts',(0.00802138847203439,-1.19442331774104,
-2.85415543927884E-6));
#9563=CARTESIAN_POINT('Ctrl Pts',(0.0128049030182357,-1.21185152247087,
-2.04128886843626E-6));
#9564=CARTESIAN_POINT('Ctrl Pts',(0.0191087770915565,-1.22877027194193,
1.71240493184593E-7));
#9565=CARTESIAN_POINT('Ctrl Pts',(0.0202201941454154,-1.23175316571065,
5.613248819379E-7));
#9566=CARTESIAN_POINT('Ctrl Pts',(0.0213789882593307,-1.23472016785247,
9.85829603970989E-7));
#9567=CARTESIAN_POINT('Ctrl Pts',(0.0225850188675993,-1.23766995297306,
1.43287414332239E-6));
#9568=CARTESIAN_POINT('Ctrl Pts',(0.0294291562303479,-1.25440977235863,
3.96981990042924E-6));
#9569=CARTESIAN_POINT('Ctrl Pts',(0.0377300686697735,-1.27044838970616,
7.55798501181421E-6));
#9570=CARTESIAN_POINT('Ctrl Pts',(0.0474121614036163,-1.28556782977674,
8.05058320302158E-6));
#9571=CARTESIAN_POINT('Ctrl Pts',(0.0511425121829324,-1.29139310088294,
8.24037316857697E-6));
#9572=CARTESIAN_POINT('Ctrl Pts',(0.0550784035723718,-1.29708174651376,
7.93435480917585E-6));
#9573=CARTESIAN_POINT('Ctrl Pts',(0.0592173503759339,-1.30262033374061,
6.74858081742264E-6));
#9574=CARTESIAN_POINT('Ctrl Pts',(0.0675201807396794,-1.31373087764993,
4.36988865960166E-6));
#9575=CARTESIAN_POINT('Ctrl Pts',(0.0766394565597649,-1.32423847988766,
-1.46587651676554E-6));
#9576=CARTESIAN_POINT('Ctrl Pts',(0.0864911062490747,-1.33409287340636,
-7.46705500292641E-6));
#9577=CARTESIAN_POINT('Ctrl Pts',(0.0992988409846585,-1.34690417528452,
-1.52689465211603E-5));
#9578=CARTESIAN_POINT('Ctrl Pts',(0.113232871116931,-1.35850278376499,-2.31308069859054E-5));
#9579=CARTESIAN_POINT('Ctrl Pts',(0.128081622025101,-1.36880445085772,-2.72849174168177E-5));
#9580=CARTESIAN_POINT('Ctrl Pts',(0.142447925282442,-1.37877140864598,-3.13040575171566E-5));
#9581=CARTESIAN_POINT('Ctrl Pts',(0.157671864768995,-1.38752483454192,-3.1899138628041E-5));
#9582=CARTESIAN_POINT('Ctrl Pts',(0.173588691395025,-1.39495074934422,-2.90326641197332E-5));
#9583=CARTESIAN_POINT('Ctrl Pts',(0.189936400238013,-1.40257769006131,-2.60885916756054E-5));
#9584=CARTESIAN_POINT('Ctrl Pts',(0.206881864105471,-1.40874232120582,-1.95409011442111E-5));
#9585=CARTESIAN_POINT('Ctrl Pts',(0.22423558959196,-1.41334558507228,-1.29462590315495E-5));
#9586=CARTESIAN_POINT('Ctrl Pts',(0.241260467995769,-1.4178616186841,-6.47658310103417E-6));
#9587=CARTESIAN_POINT('Ctrl Pts',(0.258679581942429,-1.42087546890512,-1.12101563992788E-10));
#9588=CARTESIAN_POINT('Ctrl Pts',(0.27632692456468,-1.42224670711126,1.05818132034585E-16));
#9589=CARTESIAN_POINT('',(0.,-1.4,0.));
#9590=CARTESIAN_POINT('',(0.292382661757373,-1.22257596919059,0.));
#9591=CARTESIAN_POINT('Ctrl Pts',(0.200274469199584,-1.12301388185427,-2.68882138776405E-17));
#9592=CARTESIAN_POINT('Ctrl Pts',(0.200274469314753,-1.13095194822878,-2.85686379674833E-12));
#9593=CARTESIAN_POINT('Ctrl Pts',(0.201244085522878,-1.13884856843413,-1.08105759021766E-6));
#9594=CARTESIAN_POINT('Ctrl Pts',(0.203110344361254,-1.14653799330522,-1.10782444979703E-6));
#9595=CARTESIAN_POINT('Ctrl Pts',(0.204308287281872,-1.15147379958167,-1.12500597321754E-6));
#9596=CARTESIAN_POINT('Ctrl Pts',(0.205876831658669,-1.15632444796435,-7.573778542164E-7));
#9597=CARTESIAN_POINT('Ctrl Pts',(0.207807574899602,-1.16104329283393,-1.57887042599725E-7));
#9598=CARTESIAN_POINT('Ctrl Pts',(0.21096922807971,-1.1687705506961,8.23798139982571E-7));
#9599=CARTESIAN_POINT('Ctrl Pts',(0.215060220496011,-1.17605061753432,2.67511715935828E-6));
#9600=CARTESIAN_POINT('Ctrl Pts',(0.220020901709485,-1.18268777995331,1.20301732358232E-6));
#9601=CARTESIAN_POINT('Ctrl Pts',(0.222788929945646,-1.18639127392786,3.81595076007225E-7));
#9602=CARTESIAN_POINT('Ctrl Pts',(0.225828882930032,-1.18989419630164,-1.55522758636672E-6));
#9603=CARTESIAN_POINT('Ctrl Pts',(0.229112809647272,-1.19317965616817,-3.52099818518546E-6));
#9604=CARTESIAN_POINT('Ctrl Pts',(0.234731790749985,-1.1988012605745,-6.88454091865859E-6));
#9605=CARTESIAN_POINT('Ctrl Pts',(0.240999377733319,-1.20372479786492,-1.00686973618824E-5));
#9606=CARTESIAN_POINT('Ctrl Pts',(0.247759525934523,-1.2078808899968,-1.07387199666626E-5));
#9607=CARTESIAN_POINT('Ctrl Pts',(0.251104201987095,-1.20993717358883,-1.10702228411842E-5));
#9608=CARTESIAN_POINT('Ctrl Pts',(0.254570062984725,-1.21180502729412,-1.08478245319173E-5));
#9609=CARTESIAN_POINT('Ctrl Pts',(0.258140701417296,-1.21347208138814,-1.01264154182862E-5));
#9610=CARTESIAN_POINT('Ctrl Pts',(0.265309933881728,-1.21681924144269,-8.67794906268977E-6));
#9611=CARTESIAN_POINT('Ctrl Pts',(0.27282354441991,-1.21932394229889,-5.03816435877804E-6));
#9612=CARTESIAN_POINT('Ctrl Pts',(0.280540402387729,-1.22090470300999,-2.38011023443526E-6));
#9613=CARTESIAN_POINT('Ctrl Pts',(0.284441227387562,-1.22170376798259,-1.03647996128718E-6));
#9614=CARTESIAN_POINT('Ctrl Pts',(0.288394358015454,-1.22226603782358,-8.41267709508591E-12));
#9615=CARTESIAN_POINT('Ctrl Pts',(0.292382661757373,-1.22257596919059,3.10081821330854E-17));
#9616=CARTESIAN_POINT('',(0.9,-1.266106713614,0.));
#9617=CARTESIAN_POINT('Ctrl Pts',(0.29238266175737,-1.22257596919059,3.4274341177698E-16));
#9618=CARTESIAN_POINT('Ctrl Pts',(0.494894519961671,-1.23831317320793,3.6654050078524E-12));
#9619=CARTESIAN_POINT('Ctrl Pts',(0.697432753591781,-1.25280566766171,-2.10377631034678E-8));
#9620=CARTESIAN_POINT('Ctrl Pts',(0.900000000000002,-1.266106713614,4.80511808774455E-17));
#9621=CARTESIAN_POINT('',(0.9,1.34328341716202,0.));
#9622=CARTESIAN_POINT('',(3.5,-1.37552980833516,0.));
#9623=CARTESIAN_POINT('Ctrl Pts',(1.10000000028363,-1.27885335028943,-5.13283219638443E-11));
#9624=CARTESIAN_POINT('Ctrl Pts',(1.8994825293422,-1.32827224294784,2.51289069808066E-7));
#9625=CARTESIAN_POINT('Ctrl Pts',(2.69943073922525,-1.35940904940056,2.35357980118634E-7));
#9626=CARTESIAN_POINT('Ctrl Pts',(3.50000000097418,-1.37552980835478,8.59034485311056E-16));
#9627=CARTESIAN_POINT('',(3.5,1.44777777777778,0.));
#9628=CARTESIAN_POINT('',(7.1,-1.35793097395724,0.));
#9629=CARTESIAN_POINT('Ctrl Pts',(3.700000000362,-1.379246395385,-6.25385501848083E-12));
#9630=CARTESIAN_POINT('Ctrl Pts',(4.26467016042339,-1.38886773733237,1.63880713394601E-8));
#9631=CARTESIAN_POINT('Ctrl Pts',(4.82965558050887,-1.39115503781354,-4.12727732537403E-8));
#9632=CARTESIAN_POINT('Ctrl Pts',(5.39500817395676,-1.38725486475042,-3.97626883737645E-8));
#9633=CARTESIAN_POINT('Ctrl Pts',(5.96336684492344,-1.38333395379258,-3.82445741104923E-8));
#9634=CARTESIAN_POINT('Ctrl Pts',(6.53173538886785,-1.37316170188981,3.71969681223073E-9));
#9635=CARTESIAN_POINT('Ctrl Pts',(7.1000000000396,-1.35793097389613,-4.88946831112289E-12));
#9636=CARTESIAN_POINT('',(7.1,1.42555555555556,0.));
#9637=CARTESIAN_POINT('',(10.2,-1.23178301601145,0.));
#9638=CARTESIAN_POINT('',(10.5052647440597,-1.21555035534119,0.));
#9639=CARTESIAN_POINT('Ctrl Pts',(10.2,-1.23178301601145,-4.56855690431079E-17));
#9640=CARTESIAN_POINT('Ctrl Pts',(10.3017652114452,-1.22646242153193,-6.28718440835499E-11));
#9641=CARTESIAN_POINT('Ctrl Pts',(10.4035203469111,-1.22104923788321,1.43982679105611E-13));
#9642=CARTESIAN_POINT('Ctrl Pts',(10.5052647440597,-1.21555035534119,6.44897004721534E-17));
#9643=CARTESIAN_POINT('',(10.5997255308004,-1.11583328740478,1.38777878078145E-17));
#9644=CARTESIAN_POINT('Ctrl Pts',(10.5052647440597,-1.21555035534119,-1.86482773667507E-17));
#9645=CARTESIAN_POINT('Ctrl Pts',(10.5131888530666,-1.21512208850275,-5.60416335832109E-13));
#9646=CARTESIAN_POINT('Ctrl Pts',(10.5210180054001,-1.21372544600509,-1.35972994235015E-6));
#9647=CARTESIAN_POINT('Ctrl Pts',(10.5285917824072,-1.2114444991589,-1.66070161277884E-6));
#9648=CARTESIAN_POINT('Ctrl Pts',(10.5334522234388,-1.20998071066451,-1.8538489757029E-6));
#9649=CARTESIAN_POINT('Ctrl Pts',(10.538207639053,-1.20815156029678,-1.66445033219183E-6));
#9650=CARTESIAN_POINT('Ctrl Pts',(10.542812250732,-1.20596855068549,-1.19054254011085E-6));
#9651=CARTESIAN_POINT('Ctrl Pts',(10.5499808226381,-1.20256998801374,-4.52751316616249E-7));
#9652=CARTESIAN_POINT('Ctrl Pts',(10.5567010840309,-1.19835579238971,1.16775294480959E-6));
#9653=CARTESIAN_POINT('Ctrl Pts',(10.5628099082467,-1.1933896765605,3.12218506849373E-7));
#9654=CARTESIAN_POINT('Ctrl Pts',(10.563392699667,-1.1929159013142,2.30599178383296E-7));
#9655=CARTESIAN_POINT('Ctrl Pts',(10.563969906567,-1.19243524850296,1.23643260424227E-7));
#9656=CARTESIAN_POINT('Ctrl Pts',(10.5645413730323,-1.19194775268147,-1.33988689923433E-8));
#9657=CARTESIAN_POINT('Ctrl Pts',(10.5677990734116,-1.18916873515523,-7.94620907596477E-7));
#9658=CARTESIAN_POINT('Ctrl Pts',(10.5708705204042,-1.18616755700159,-2.52696578471864E-6));
#9659=CARTESIAN_POINT('Ctrl Pts',(10.5737438185805,-1.18296717200411,-4.3349897000341E-6));
#9660=CARTESIAN_POINT('Ctrl Pts',(10.579054042416,-1.17705244973962,-7.67644996655303E-6));
#9661=CARTESIAN_POINT('Ctrl Pts',(10.5836289246435,-1.17052745137283,-1.0999028846932E-5));
#9662=CARTESIAN_POINT('Ctrl Pts',(10.5874112735695,-1.16355342251842,-1.18035167459916E-5));
#9663=CARTESIAN_POINT('Ctrl Pts',(10.5894705469099,-1.15975646143,-1.22415145393192E-5));
#9664=CARTESIAN_POINT('Ctrl Pts',(10.5912942421259,-1.15582570378367,-1.20038889321768E-5));
#9665=CARTESIAN_POINT('Ctrl Pts',(10.5928674986933,-1.15178403025788,-1.11465830745351E-5));
#9666=CARTESIAN_POINT('Ctrl Pts',(10.5957384082276,-1.14440870489779,-9.58215448007377E-6));
#9667=CARTESIAN_POINT('Ctrl Pts',(10.5977463817932,-1.13674651935037,-5.80208140981121E-6));
#9668=CARTESIAN_POINT('Ctrl Pts',(10.5988207707371,-1.12894377506163,-2.8960211281105E-6));
#9669=CARTESIAN_POINT('Ctrl Pts',(10.5994175893465,-1.12460938291963,-1.28171667533415E-6));
#9670=CARTESIAN_POINT('Ctrl Pts',(10.5997255306822,-1.12023121224821,-9.4020583932734E-12));
#9671=CARTESIAN_POINT('Ctrl Pts',(10.5997255308004,-1.11583328740478,-9.97465998686664E-18));
#9672=CARTESIAN_POINT('',(10.5997255308004,1.11583328740478,0.));
#9673=CARTESIAN_POINT('',(10.5997255308004,0.7,0.));
#9674=CARTESIAN_POINT('',(10.5052647440597,1.21555035534119,0.));
#9675=CARTESIAN_POINT('Ctrl Pts',(10.5997255308004,1.11583328740478,8.8037216405823E-17));
#9676=CARTESIAN_POINT('Ctrl Pts',(10.5997255307124,1.12376989384288,-2.22024716398596E-12));
#9677=CARTESIAN_POINT('Ctrl Pts',(10.5987536115518,1.13166401228391,-1.27532141444775E-6));
#9678=CARTESIAN_POINT('Ctrl Pts',(10.5968849989732,1.13935090273995,-1.5236651967046E-6));
#9679=CARTESIAN_POINT('Ctrl Pts',(10.5956849616024,1.14428748291596,-1.68315348385219E-6));
#9680=CARTESIAN_POINT('Ctrl Pts',(10.5941139374364,1.14913880701507,-1.46899737395989E-6));
#9681=CARTESIAN_POINT('Ctrl Pts',(10.5921809408638,1.1538584293407,-9.90118991603547E-7));
#9682=CARTESIAN_POINT('Ctrl Pts',(10.5891742477341,1.16119959911942,-2.45244239835432E-7));
#9683=CARTESIAN_POINT('Ctrl Pts',(10.5853292249979,1.16813727090899,1.33309554558619E-6));
#9684=CARTESIAN_POINT('Ctrl Pts',(10.5807005079991,1.17450509276749,4.08358240744415E-7));
#9685=CARTESIAN_POINT('Ctrl Pts',(10.5802604812716,1.17511044665166,3.20448539159982E-7));
#9686=CARTESIAN_POINT('Ctrl Pts',(10.5798133373602,1.17571063303672,2.07176952714776E-7));
#9687=CARTESIAN_POINT('Ctrl Pts',(10.5793591019426,1.17630549598644,6.38823567561716E-8));
#9688=CARTESIAN_POINT('Ctrl Pts',(10.5767566952267,1.17971358631841,-7.57081408668461E-7));
#9689=CARTESIAN_POINT('Ctrl Pts',(10.5739217504488,1.18294722379721,-2.53660858190298E-6));
#9690=CARTESIAN_POINT('Ctrl Pts',(10.570876618072,1.18599321478588,-4.38998728286835E-6));
#9691=CARTESIAN_POINT('Ctrl Pts',(10.5652565693637,1.19161484813492,-7.81055403847458E-6));
#9692=CARTESIAN_POINT('Ctrl Pts',(10.5589874561388,1.19653507038546,-1.11999964534866E-5));
#9693=CARTESIAN_POINT('Ctrl Pts',(10.5522271124844,1.20068789486255,-1.20263298844839E-5));
#9694=CARTESIAN_POINT('Ctrl Pts',(10.5485500617744,1.20294667739977,-1.24757848359648E-5));
#9695=CARTESIAN_POINT('Ctrl Pts',(10.5447269560479,1.20497781184918,-1.22374322375965E-5));
#9696=CARTESIAN_POINT('Ctrl Pts',(10.5407797717187,1.20676523914267,-1.13674773191707E-5));
#9697=CARTESIAN_POINT('Ctrl Pts',(10.5335711832013,1.210029547771,-9.77871264224002E-6));
#9698=CARTESIAN_POINT('Ctrl Pts',(10.5260296312848,1.21244761587922,-5.9245235663186E-6));
#9699=CARTESIAN_POINT('Ctrl Pts',(10.5182973307397,1.21394093281975,-2.95733858081469E-6));
#9700=CARTESIAN_POINT('Ctrl Pts',(10.514004731837,1.21476995008607,-1.31010113336685E-6));
#9701=CARTESIAN_POINT('Ctrl Pts',(10.5096528988527,1.21531319279956,-7.28166367327128E-12));
#9702=CARTESIAN_POINT('Ctrl Pts',(10.5052647440597,1.21555035534119,-3.31765864780564E-17));
#9703=CARTESIAN_POINT('',(10.2,1.23178301601145,0.));
#9704=CARTESIAN_POINT('Ctrl Pts',(10.5052647440597,1.21555035534119,1.20285454773689E-16));
#9705=CARTESIAN_POINT('Ctrl Pts',(10.4035203468995,1.22104923788384,1.44021921739714E-13));
#9706=CARTESIAN_POINT('Ctrl Pts',(10.3017652114309,1.22646242153268,-6.28696045710378E-11));
#9707=CARTESIAN_POINT('Ctrl Pts',(10.2,1.23178301601145,1.23125603768043E-16));
#9708=CARTESIAN_POINT('',(10.2,-1.30754691548544,0.));
#9709=CARTESIAN_POINT('Origin',(8.8,0.,0.));
#9710=CARTESIAN_POINT('',(8.4,-4.89858719658942E-17,0.));
#9711=CARTESIAN_POINT('Origin',(2.,0.,0.));
#9712=CARTESIAN_POINT('',(1.6,-4.89858719658941E-17,0.7));
#9713=CARTESIAN_POINT('Origin',(2.,0.,0.7));
#9714=CARTESIAN_POINT('',(1.6,-4.89858719658941E-17,0.));
#9715=CARTESIAN_POINT('Origin',(10.2,-1.30754691548544,0.));
#9716=CARTESIAN_POINT('',(10.1999999975107,-1.19856231453552,0.605472757505173));
#9717=CARTESIAN_POINT('Ctrl Pts',(10.2,-1.23178301601145,0.));
#9718=CARTESIAN_POINT('Ctrl Pts',(10.2,-1.22625045235593,0.100869147801815));
#9719=CARTESIAN_POINT('Ctrl Pts',(10.2,-1.22071692450357,0.201739022585575));
#9720=CARTESIAN_POINT('Ctrl Pts',(10.2,-1.2096433936729,0.403562754186249));
#9721=CARTESIAN_POINT('Ctrl Pts',(10.1999999975107,-1.20410330368611,0.50451817268257));
#9722=CARTESIAN_POINT('Ctrl Pts',(10.1999999975107,-1.19856231453552,0.605472757505173));
#9723=CARTESIAN_POINT('',(10.1999999975107,1.19856231453552,0.605472757505173));
#9724=CARTESIAN_POINT('Ctrl Pts',(10.1999999975107,1.19856231453552,0.605472757505173));
#9725=CARTESIAN_POINT('Ctrl Pts',(10.1999999975107,1.20410418062036,0.504502195294633));
#9726=CARTESIAN_POINT('Ctrl Pts',(10.2,1.20964514726505,0.403530798997214));
#9727=CARTESIAN_POINT('Ctrl Pts',(10.2,1.22071867750565,0.201707067365009));
#9728=CARTESIAN_POINT('Ctrl Pts',(10.2,1.22625132869937,0.100853170395858));
#9729=CARTESIAN_POINT('Ctrl Pts',(10.2,1.23178301601145,0.));
#9730=CARTESIAN_POINT('',(10.1999999980542,1.09857320530976,0.7));
#9731=CARTESIAN_POINT('Ctrl Pts',(10.1999999999973,1.09857320510493,0.7));
#9732=CARTESIAN_POINT('Ctrl Pts',(10.2000000008642,1.10649088744708,0.699999999248278));
#9733=CARTESIAN_POINT('Ctrl Pts',(10.1999989363772,1.11434529358656,0.699006164779054));
#9734=CARTESIAN_POINT('Ctrl Pts',(10.1999980093114,1.12199598895487,0.697118997523365));
#9735=CARTESIAN_POINT('Ctrl Pts',(10.1999974900707,1.12628106973794,0.696062013320951));
#9736=CARTESIAN_POINT('Ctrl Pts',(10.1999970168623,1.13050229860485,0.694723760583242));
#9737=CARTESIAN_POINT('Ctrl Pts',(10.199996713894,1.13463332887353,0.693115046692397));
#9738=CARTESIAN_POINT('Ctrl Pts',(10.1999961690675,1.14206214329588,0.690222103243312));
#9739=CARTESIAN_POINT('Ctrl Pts',(10.1999962772589,1.14911941279843,0.686488866209959));
#9740=CARTESIAN_POINT('Ctrl Pts',(10.1999969599022,1.15565885618684,0.681996408643444));
#9741=CARTESIAN_POINT('Ctrl Pts',(10.1999973343062,1.15924549304116,0.679532465931891));
#9742=CARTESIAN_POINT('Ctrl Pts',(10.1999978674396,1.16267609380848,0.676839263748528));
#9743=CARTESIAN_POINT('Ctrl Pts',(10.1999983417863,1.16592263776853,0.673924718551186));
#9744=CARTESIAN_POINT('Ctrl Pts',(10.199998806773,1.16910511991263,0.671067684066867));
#9745=CARTESIAN_POINT('Ctrl Pts',(10.1999992207276,1.17209141256199,0.668015240668471));
#9746=CARTESIAN_POINT('Ctrl Pts',(10.1999992206607,1.17485880184773,0.664778864469812));
#9747=CARTESIAN_POINT('Ctrl Pts',(10.1999992205369,1.17997899231675,0.658790960038769));
#9748=CARTESIAN_POINT('Ctrl Pts',(10.1999979581638,1.18435276586188,0.652174799271591));
#9749=CARTESIAN_POINT('Ctrl Pts',(10.1999975326045,1.18791964688485,0.645095405674036));
#9750=CARTESIAN_POINT('Ctrl Pts',(10.1999974898604,1.18827791229431,0.644384335742179));
#9751=CARTESIAN_POINT('Ctrl Pts',(10.1999974535047,1.18862799840101,0.643668573506599));
#9752=CARTESIAN_POINT('Ctrl Pts',(10.1999974242393,1.18896981696374,0.64294827577739));
#9753=CARTESIAN_POINT('Ctrl Pts',(10.1999971329942,1.1923715530028,0.635779961907205));
#9754=CARTESIAN_POINT('Ctrl Pts',(10.1999977790614,1.19491900203126,0.628247233077589));
#9755=CARTESIAN_POINT('Ctrl Pts',(10.1999987199397,1.19655829940385,0.620518158911201));
#9756=CARTESIAN_POINT('Ctrl Pts',(10.1999993222661,1.19760773597399,0.615570201805241));
#9757=CARTESIAN_POINT('Ctrl Pts',(10.2,1.19828413277105,0.610541112135461));
#9758=CARTESIAN_POINT('Ctrl Pts',(10.2,1.19856231427281,0.60547275750556));
#9759=CARTESIAN_POINT('',(10.2,-1.09857320510402,0.7));
#9760=CARTESIAN_POINT('',(10.2,-0.653773457742722,0.7));
#9761=CARTESIAN_POINT('Ctrl Pts',(10.2,-1.19856231427281,0.60547275750556));
#9762=CARTESIAN_POINT('Ctrl Pts',(10.2,-1.19812809376428,0.613384079828744));
#9763=CARTESIAN_POINT('Ctrl Pts',(10.1999984889428,-1.1967261327477,0.621202329970501));
#9764=CARTESIAN_POINT('Ctrl Pts',(10.1999978161146,-1.19444079525024,0.628767398200536));
#9765=CARTESIAN_POINT('Ctrl Pts',(10.1999974438306,-1.19317629038787,0.632953241898348));
#9766=CARTESIAN_POINT('Ctrl Pts',(10.1999972759003,-1.19164034846853,0.637061602680377));
#9767=CARTESIAN_POINT('Ctrl Pts',(10.1999973648938,-1.18984073583679,0.641063423920242));
#9768=CARTESIAN_POINT('Ctrl Pts',(10.1999975257516,-1.18658789218766,0.648296813248274));
#9769=CARTESIAN_POINT('Ctrl Pts',(10.1999986492083,-1.18251199594868,0.655103972585077));
#9770=CARTESIAN_POINT('Ctrl Pts',(10.1999990866637,-1.1776776067306,0.66132208754656));
#9771=CARTESIAN_POINT('Ctrl Pts',(10.1999991692372,-1.17676507450965,0.662495809810115));
#9772=CARTESIAN_POINT('Ctrl Pts',(10.1999992204458,-1.17582538639523,0.663648473741297));
#9773=CARTESIAN_POINT('Ctrl Pts',(10.1999992199672,-1.17485880188435,0.664778864469789));
#9774=CARTESIAN_POINT('Ctrl Pts',(10.1999992190419,-1.17299032792757,0.666963987046661));
#9775=CARTESIAN_POINT('Ctrl Pts',(10.1999990265713,-1.17102137903347,0.669065925022507));
#9776=CARTESIAN_POINT('Ctrl Pts',(10.1999987631451,-1.16895889720817,0.671081139337088));
#9777=CARTESIAN_POINT('Ctrl Pts',(10.1999980371048,-1.16327440276409,0.676635357771578));
#9778=CARTESIAN_POINT('Ctrl Pts',(10.1999968952367,-1.15694629605269,0.681471105251756));
#9779=CARTESIAN_POINT('Ctrl Pts',(10.1999965193249,-1.15013861030111,0.685534582868085));
#9780=CARTESIAN_POINT('Ctrl Pts',(10.1999962798276,-1.14580136285465,0.688123466749966));
#9781=CARTESIAN_POINT('Ctrl Pts',(10.1999963003895,-1.14126848503633,0.690398200126003));
#9782=CARTESIAN_POINT('Ctrl Pts',(10.1999965837416,-1.13657664085124,0.692335536714198));
#9783=CARTESIAN_POINT('Ctrl Pts',(10.199997026059,-1.12925259320479,0.695359751696499));
#9784=CARTESIAN_POINT('Ctrl Pts',(10.1999981114625,-1.12162598460505,0.697529439192009));
#9785=CARTESIAN_POINT('Ctrl Pts',(10.1999989867727,-1.11384404680861,0.698775198878229));
#9786=CARTESIAN_POINT('Ctrl Pts',(10.1999995533653,-1.10880676031141,0.699581585232154));
#9787=CARTESIAN_POINT('Ctrl Pts',(10.200000000559,-1.10370379302489,0.699999999512891));
#9788=CARTESIAN_POINT('Ctrl Pts',(10.1999999999973,-1.09857320510493,0.7));
#9789=CARTESIAN_POINT('Ctrl Pts',(10.0273290644374,-1.24073895154929,-0.000342977371441382));
#9790=CARTESIAN_POINT('Ctrl Pts',(10.0182194939277,-1.2301570933055,0.201590462913323));
#9791=CARTESIAN_POINT('Ctrl Pts',(10.0091098064739,-1.21957524432673,0.403523898419685));
#9792=CARTESIAN_POINT('Ctrl Pts',(10.,-1.20899340483173,0.605457329065658));
#9793=CARTESIAN_POINT('Ctrl Pts',(9.11786336174441,-1.287320026752,-0.000205293215301774));
#9794=CARTESIAN_POINT('Ctrl Pts',(9.11054075262461,-1.27673792859995,0.201728409731728));
#9795=CARTESIAN_POINT('Ctrl Pts',(9.10321803982027,-1.2661558351744,0.403662109352091));
#9796=CARTESIAN_POINT('Ctrl Pts',(9.09589522044064,-1.25557375159922,0.605595805683776));
#9797=CARTESIAN_POINT('Ctrl Pts',(8.20875307681921,-1.32613868191631,-8.19769783003664E-5));
#9798=CARTESIAN_POINT('Ctrl Pts',(8.20321812688803,-1.31555630757271,0.201851960079368));
#9799=CARTESIAN_POINT('Ctrl Pts',(8.19768309032111,-1.30497393555236,0.403785895133155));
#9800=CARTESIAN_POINT('Ctrl Pts',(8.19214796413157,-1.29439157095064,0.605719828258773));
#9801=CARTESIAN_POINT('Ctrl Pts',(7.29999999999999,-1.35236351479115,1.04083408558608E-17));
#9802=CARTESIAN_POINT('Ctrl Pts',(7.29625341766944,-1.34178092325774,0.201934092022114));
#9803=CARTESIAN_POINT('Ctrl Pts',(7.2925067690755,-1.33119833465137,0.403868182971915));
#9804=CARTESIAN_POINT('Ctrl Pts',(7.28876005303739,-1.32061574904145,0.605802272831199));
#9805=CARTESIAN_POINT('Ctrl Pts',(7.29999999953094,-1.32031613471704,0.605285370449856));
#9806=CARTESIAN_POINT('Ctrl Pts',(8.20058408060299,-1.29406305600824,0.605326635812744));
#9807=CARTESIAN_POINT('Ctrl Pts',(9.10058974048747,-1.25534320916473,0.605388449123016));
#9808=CARTESIAN_POINT('Ctrl Pts',(9.99999999968202,-1.20899340489109,0.605457329065633));
#9809=CARTESIAN_POINT('Ctrl Pts',(10.5052670937641,-1.21555282972197,-4.72190879230918E-5));
#9810=CARTESIAN_POINT('Ctrl Pts',(10.4952228315222,-1.20497561405085,0.201799837144789));
#9811=CARTESIAN_POINT('Ctrl Pts',(10.4851784461209,-1.19439840869387,0.403646887802288));
#9812=CARTESIAN_POINT('Ctrl Pts',(10.4751339353761,-1.18382121389426,0.605493932788863));
#9813=CARTESIAN_POINT('Ctrl Pts',(10.4035069533234,-1.22105168617584,-3.13467776074076E-5));
#9814=CARTESIAN_POINT('Ctrl Pts',(10.3936624949941,-1.21047444506522,0.201815739766394));
#9815=CARTESIAN_POINT('Ctrl Pts',(10.3838179147697,-1.19989721405033,0.403662820908308));
#9816=CARTESIAN_POINT('Ctrl Pts',(10.3739732104882,-1.18931999337004,0.605509896555428));
#9817=CARTESIAN_POINT('Ctrl Pts',(10.3017512542637,-1.22646400658821,-1.55943981238903E-5));
#9818=CARTESIAN_POINT('Ctrl Pts',(10.2921066085356,-1.21588673949083,0.201831522212972));
#9819=CARTESIAN_POINT('Ctrl Pts',(10.2824618422276,-1.20530948226626,0.403678633593635));
#9820=CARTESIAN_POINT('Ctrl Pts',(10.2728169532007,-1.19473223514815,0.605525739654126));
#9821=CARTESIAN_POINT('Ctrl Pts',(10.2,-1.23178301601145,-4.5102810375397E-17));
#9822=CARTESIAN_POINT('Ctrl Pts',(10.1905551755811,-1.22120572247414,0.20184714636246));
#9823=CARTESIAN_POINT('Ctrl Pts',(10.1811102319487,-1.21062843858304,0.403694287664275));
#9824=CARTESIAN_POINT('Ctrl Pts',(10.1716651669877,-1.20005116456574,0.605541423818621));
#9825=CARTESIAN_POINT('',(10.4735630903435,-1.18390659316268,0.605494180667944));
#9826=CARTESIAN_POINT('Ctrl Pts',(10.1999999975038,-1.19856231440453,0.605472757505366));
#9827=CARTESIAN_POINT('Ctrl Pts',(10.2911933328565,-1.19375025772558,0.605479840815741));
#9828=CARTESIAN_POINT('Ctrl Pts',(10.3823809652617,-1.18886335120032,0.605486986548286));
#9829=CARTESIAN_POINT('Ctrl Pts',(10.4735630903435,-1.18390659316268,0.605494180667944));
#9830=CARTESIAN_POINT('Ctrl Pts',(10.4735630903435,-1.18390659316268,0.605494180667945));
#9831=CARTESIAN_POINT('Ctrl Pts',(10.4841302498201,-1.19445434834508,0.403662775875149));
#9832=CARTESIAN_POINT('Ctrl Pts',(10.4946974680575,-1.20500226999407,0.201831382381129));
#9833=CARTESIAN_POINT('Ctrl Pts',(10.5052647440597,-1.21555035534119,-6.86299975183324E-17));
#9834=CARTESIAN_POINT('Ctrl Pts',(10.,-1.10900986674273,0.7));
#9835=CARTESIAN_POINT('Ctrl Pts',(9.09944331332257,-1.15544418981837,0.7));
#9836=CARTESIAN_POINT('Ctrl Pts',(8.1984670949788,-1.19422430779862,0.7));
#9837=CARTESIAN_POINT('Ctrl Pts',(7.29709043526679,-1.22049830417059,0.7));
#9838=CARTESIAN_POINT('Ctrl Pts',(10.0014871213396,-1.13785139984992,0.7));
#9839=CARTESIAN_POINT('Ctrl Pts',(9.10076698492608,-1.18430758604571,0.700000491839571));
#9840=CARTESIAN_POINT('Ctrl Pts',(8.19957769811723,-1.22310890030201,0.699999704549177));
#9841=CARTESIAN_POINT('Ctrl Pts',(7.29793284700475,-1.24939875264889,0.7));
#9842=CARTESIAN_POINT('Ctrl Pts',(10.0040646682326,-1.18784086746588,0.676686753673613));
#9843=CARTESIAN_POINT('Ctrl Pts',(9.10306300621911,-1.23433322993607,0.676664155483858));
#9844=CARTESIAN_POINT('Ctrl Pts',(8.20149954052229,-1.27317186922949,0.676644146017133));
#9845=CARTESIAN_POINT('Ctrl Pts',(7.29939288958795,-1.29948813715084,0.676630595533454));
#9846=CARTESIAN_POINT('Ctrl Pts',(10.0050807923581,-1.20754778500352,0.627085325222079));
#9847=CARTESIAN_POINT('Ctrl Pts',(9.10396596140607,-1.25402923300358,0.627026849623412));
#9848=CARTESIAN_POINT('Ctrl Pts',(8.20225661204673,-1.29285896783792,0.626974637782525));
#9849=CARTESIAN_POINT('Ctrl Pts',(7.29996660609514,-1.31917051289423,0.626939603849942));
#9850=CARTESIAN_POINT('Ctrl Pts',(10.0051416645797,-1.20872835322339,0.605457722909465));
#9851=CARTESIAN_POINT('Ctrl Pts',(9.1040197884667,-1.25519559703033,0.605388684776982));
#9852=CARTESIAN_POINT('Ctrl Pts',(8.20230020786566,-1.29401302889245,0.605326714446839));
#9853=CARTESIAN_POINT('Ctrl Pts',(7.29999999953094,-1.32031613471704,0.605285370449856));
#9854=CARTESIAN_POINT('Ctrl Pts',(10.4681436286308,-1.08420482079362,0.7));
#9855=CARTESIAN_POINT('Ctrl Pts',(10.3770124662346,-1.0891584122264,0.7));
#9856=CARTESIAN_POINT('Ctrl Pts',(10.285877616441,-1.09404209584202,0.7));
#9857=CARTESIAN_POINT('Ctrl Pts',(10.1947388861048,-1.09885088260188,0.7));
#9858=CARTESIAN_POINT('Ctrl Pts',(10.4697107510168,-1.11303515260326,0.7));
#9859=CARTESIAN_POINT('Ctrl Pts',(10.3785648662465,-1.11799094453753,0.700000051218742));
#9860=CARTESIAN_POINT('Ctrl Pts',(10.2874149314686,-1.12287675076168,0.699999949550842));
#9861=CARTESIAN_POINT('Ctrl Pts',(10.196260416419,-1.12768774893097,0.7));
#9862=CARTESIAN_POINT('Ctrl Pts',(10.4724269697127,-1.16300539549315,0.676698381019543));
#9863=CARTESIAN_POINT('Ctrl Pts',(10.3812557252598,-1.16796482352885,0.676696026813929));
#9864=CARTESIAN_POINT('Ctrl Pts',(10.2900793016129,-1.17285439035486,0.676693724638983));
#9865=CARTESIAN_POINT('Ctrl Pts',(10.1988975981852,-1.17766904563614,0.67669140632491));
#9866=CARTESIAN_POINT('Ctrl Pts',(10.4734985149421,-1.18271860027509,0.627116141711795));
#9867=CARTESIAN_POINT('Ctrl Pts',(10.382317043787,-1.18767684023183,0.627110048826767));
#9868=CARTESIAN_POINT('Ctrl Pts',(10.2911301919381,-1.19256517083271,0.627104033151799));
#9869=CARTESIAN_POINT('Ctrl Pts',(10.1999375452555,-1.19737868557977,0.627098033786781));
#9870=CARTESIAN_POINT('Ctrl Pts',(10.4735630903435,-1.18390659316268,0.605494180667944));
#9871=CARTESIAN_POINT('Ctrl Pts',(10.3823809652617,-1.18886335120032,0.605486986548286));
#9872=CARTESIAN_POINT('Ctrl Pts',(10.2911933328565,-1.19375025772558,0.605479840815741));
#9873=CARTESIAN_POINT('Ctrl Pts',(10.1999999975038,-1.19856231440453,0.605472757505366));
#9874=CARTESIAN_POINT('',(10.4681436258201,-1.08420482094639,0.7));
#9875=CARTESIAN_POINT('Ctrl Pts',(10.4681436258201,-1.0842048209464,0.7));
#9876=CARTESIAN_POINT('Ctrl Pts',(10.3787660248044,-1.08906309452597,0.7));
#9877=CARTESIAN_POINT('Ctrl Pts',(10.289384876933,-1.09385412476048,0.7));
#9878=CARTESIAN_POINT('Ctrl Pts',(10.1999999999973,-1.09857320510493,0.7));
#9879=CARTESIAN_POINT('Origin',(10.4681436286308,-1.08420482099672,0.6));
#9880=CARTESIAN_POINT('Origin',(5.4,-8.11656130105013E-18,0.7));
#9881=CARTESIAN_POINT('',(10.4681436286308,1.08420482109828,0.7));
#9882=CARTESIAN_POINT('Ctrl Pts',(10.1999999980461,1.09857320520795,0.7));
#9883=CARTESIAN_POINT('Ctrl Pts',(10.2893848765692,1.09385412478074,0.7));
#9884=CARTESIAN_POINT('Ctrl Pts',(10.3787660260279,1.08906309446088,0.7));
#9885=CARTESIAN_POINT('Ctrl Pts',(10.4681436286308,1.08420482079361,0.7));
#9886=CARTESIAN_POINT('',(10.4681436286308,0.7,0.7));
#9887=CARTESIAN_POINT('Ctrl Pts',(7.3,1.35236351479305,-3.57463069561303E-11));
#9888=CARTESIAN_POINT('Ctrl Pts',(7.29625341766908,1.34178092325856,0.20193409200674));
#9889=CARTESIAN_POINT('Ctrl Pts',(7.29250676907475,1.33119833465113,0.403868182976914));
#9890=CARTESIAN_POINT('Ctrl Pts',(7.28876005303626,1.32061574904014,0.60580227285657));
#9891=CARTESIAN_POINT('Ctrl Pts',(8.20875307682014,1.32613868191819,-8.19770140467192E-5));
#9892=CARTESIAN_POINT('Ctrl Pts',(8.20321812688841,1.31555630757352,0.201851960063995));
#9893=CARTESIAN_POINT('Ctrl Pts',(8.19768309032092,1.3049739355521,0.403785895138154));
#9894=CARTESIAN_POINT('Ctrl Pts',(8.19214796413082,1.29439157094932,0.605719828284144));
#9895=CARTESIAN_POINT('Ctrl Pts',(9.11786336174626,1.28732002675385,-0.000205293251048056));
#9896=CARTESIAN_POINT('Ctrl Pts',(9.11054075262572,1.27673792860073,0.201728409716354));
#9897=CARTESIAN_POINT('Ctrl Pts',(9.10321803982063,1.26615583517412,0.403662109357089));
#9898=CARTESIAN_POINT('Ctrl Pts',(9.09589522044026,1.25557375159787,0.605595805709147));
#9899=CARTESIAN_POINT('Ctrl Pts',(10.0273290644402,1.2407389515511,-0.000342977407187712));
#9900=CARTESIAN_POINT('Ctrl Pts',(10.0182194939295,1.23015709330624,0.201590462897949));
#9901=CARTESIAN_POINT('Ctrl Pts',(10.0091098064748,1.21957524432641,0.403523898424684));
#9902=CARTESIAN_POINT('Ctrl Pts',(10.,1.20899340483035,0.605457329091028));
#9903=CARTESIAN_POINT('Ctrl Pts',(10.2,1.23178301601276,-2.39624899783797E-11));
#9904=CARTESIAN_POINT('Ctrl Pts',(10.1905551755807,1.22120572247504,0.201847146346486));
#9905=CARTESIAN_POINT('Ctrl Pts',(10.1811102319479,1.21062843858352,0.403694287656288));
#9906=CARTESIAN_POINT('Ctrl Pts',(10.1716651669865,1.2000511645658,0.605541423818621));
#9907=CARTESIAN_POINT('Ctrl Pts',(10.3017512542641,1.22646400658951,-1.55944220863836E-5));
#9908=CARTESIAN_POINT('Ctrl Pts',(10.2921066085356,1.2158867394917,0.201831522196997));
#9909=CARTESIAN_POINT('Ctrl Pts',(10.2824618422272,1.20530948226672,0.403678633585648));
#9910=CARTESIAN_POINT('Ctrl Pts',(10.2728169531999,1.19473223514819,0.605525739654127));
#9911=CARTESIAN_POINT('Ctrl Pts',(10.4035069533242,1.22105168617711,-3.13468015701665E-5));
#9912=CARTESIAN_POINT('Ctrl Pts',(10.3936624949945,1.21047444506608,0.201815739750419));
#9913=CARTESIAN_POINT('Ctrl Pts',(10.3838179147698,1.19989721405077,0.40366282090032));
#9914=CARTESIAN_POINT('Ctrl Pts',(10.3739732104878,1.18931999337006,0.605509896555428));
#9915=CARTESIAN_POINT('Ctrl Pts',(10.5052670937653,1.21555282972323,-4.72191118859062E-5));
#9916=CARTESIAN_POINT('Ctrl Pts',(10.495222831523,1.20497561405169,0.201799837128814));
#9917=CARTESIAN_POINT('Ctrl Pts',(10.4851784461213,1.19439840869429,0.403646887794301));
#9918=CARTESIAN_POINT('Ctrl Pts',(10.4751339353761,1.18382121389426,0.605493932788864));
#9919=CARTESIAN_POINT('',(10.4735630903435,1.18390659316268,0.605494180667944));
#9920=CARTESIAN_POINT('Ctrl Pts',(10.5052647440597,1.21555035534119,-4.0462425077159E-16));
#9921=CARTESIAN_POINT('Ctrl Pts',(10.4946974680575,1.20500226999407,0.201831382381129));
#9922=CARTESIAN_POINT('Ctrl Pts',(10.4841302498201,1.19445434834508,0.40366277587515));
#9923=CARTESIAN_POINT('Ctrl Pts',(10.4735630903435,1.18390659316268,0.605494180667945));
#9924=CARTESIAN_POINT('Ctrl Pts',(10.4735630903435,1.18390659316268,0.605494180667944));
#9925=CARTESIAN_POINT('Ctrl Pts',(10.3823809652617,1.18886335120032,0.605486986548286));
#9926=CARTESIAN_POINT('Ctrl Pts',(10.2911933328565,1.19375025772558,0.605479840815741));
#9927=CARTESIAN_POINT('Ctrl Pts',(10.1999999975038,1.19856231440453,0.605472757505366));
#9928=CARTESIAN_POINT('Origin',(7.1,1.42555555555556,0.));
#9929=CARTESIAN_POINT('',(7.0999999994629,-1.32593912634735,0.605276549957215));
#9930=CARTESIAN_POINT('Ctrl Pts',(7.0999999994629,-1.32593912634735,0.605276549957215));
#9931=CARTESIAN_POINT('Ctrl Pts',(7.0999999994629,-1.33126650931098,0.504490734647167));
#9932=CARTESIAN_POINT('Ctrl Pts',(7.1,-1.33659376385849,0.403703958452373));
#9933=CARTESIAN_POINT('Ctrl Pts',(7.1,-1.3472576786761,0.201945747207886));
#9934=CARTESIAN_POINT('Ctrl Pts',(7.1,-1.35259443928223,0.100972400854069));
#9935=CARTESIAN_POINT('Ctrl Pts',(7.1,-1.35793097395724,0.));
#9936=CARTESIAN_POINT('',(7.1,-1.22604182196417,0.7));
#9937=CARTESIAN_POINT('Ctrl Pts',(7.1,-1.22604182196307,0.7));
#9938=CARTESIAN_POINT('Ctrl Pts',(7.1,-1.23395163718705,0.7));
#9939=CARTESIAN_POINT('Ctrl Pts',(7.09999945440688,-1.24179783218049,0.699006056038995));
#9940=CARTESIAN_POINT('Ctrl Pts',(7.09999897931553,-1.2494401870438,0.697119011207626));
#9941=CARTESIAN_POINT('Ctrl Pts',(7.09999871186578,-1.25374240366384,0.696056710937424));
#9942=CARTESIAN_POINT('Ctrl Pts',(7.09999846845149,-1.25798007942473,0.69471034534287));
#9943=CARTESIAN_POINT('Ctrl Pts',(7.09999831430822,-1.26212651101681,0.6930909329195));
#9944=CARTESIAN_POINT('Ctrl Pts',(7.09999803835695,-1.26954956016987,0.690191818885951));
#9945=CARTESIAN_POINT('Ctrl Pts',(7.09999810102228,-1.27659977900265,0.686452252582521));
#9946=CARTESIAN_POINT('Ctrl Pts',(7.09999845706054,-1.28313109767173,0.681953977461377));
#9947=CARTESIAN_POINT('Ctrl Pts',(7.09999865314126,-1.2867280867584,0.679476645189077));
#9948=CARTESIAN_POINT('Ctrl Pts',(7.09999893113315,-1.29016742765117,0.67676830886676));
#9949=CARTESIAN_POINT('Ctrl Pts',(7.09999917787259,-1.2934208019838,0.673837071833988));
#9950=CARTESIAN_POINT('Ctrl Pts',(7.09999941835505,-1.29659167515528,0.670980166997299));
#9951=CARTESIAN_POINT('Ctrl Pts',(7.09999963169439,-1.29956664557352,0.667928795646746));
#9952=CARTESIAN_POINT('Ctrl Pts',(7.09999963110542,-1.30232317314677,0.664694459428825));
#9953=CARTESIAN_POINT('Ctrl Pts',(7.09999963001387,-1.30743194453681,0.658700148145236));
#9954=CARTESIAN_POINT('Ctrl Pts',(7.09999897381858,-1.31179333085743,0.652078782729069));
#9955=CARTESIAN_POINT('Ctrl Pts',(7.09999874753952,-1.31534789998199,0.64499600756552));
#9956=CARTESIAN_POINT('Ctrl Pts',(7.09999872438549,-1.31571162172319,0.644271261689237));
#9957=CARTESIAN_POINT('Ctrl Pts',(7.0999987046402,-1.31606685549941,0.643541664816448));
#9958=CARTESIAN_POINT('Ctrl Pts',(7.09999868869212,-1.31641350913238,0.642807383257706));
#9959=CARTESIAN_POINT('Ctrl Pts',(7.09999853283271,-1.31980133087414,0.635631300872562));
#9960=CARTESIAN_POINT('Ctrl Pts',(7.09999885939544,-1.32233451509485,0.628092322434426));
#9961=CARTESIAN_POINT('Ctrl Pts',(7.09999934101855,-1.32395982399511,0.620358959365968));
#9962=CARTESIAN_POINT('Ctrl Pts',(7.09999964997549,-1.32500244522074,0.615398075635307));
#9963=CARTESIAN_POINT('Ctrl Pts',(7.09999999934316,-1.32567060646853,0.610356529630438));
#9964=CARTESIAN_POINT('Ctrl Pts',(7.09999999981141,-1.32593912630714,0.60527654995744));
#9965=CARTESIAN_POINT('',(7.09999999995537,1.22604182196549,0.7));
#9966=CARTESIAN_POINT('',(7.1,0.712777777777778,0.7));
#9967=CARTESIAN_POINT('',(7.0999999994629,1.32593912634735,0.605276549957215));
#9968=CARTESIAN_POINT('Ctrl Pts',(7.09999999981142,1.32593912630714,0.60527654995744));
#9969=CARTESIAN_POINT('Ctrl Pts',(7.09999999908198,1.32552083177145,0.613190035045322));
#9970=CARTESIAN_POINT('Ctrl Pts',(7.09999922367565,1.32413525001942,0.621012727860624));
#9971=CARTESIAN_POINT('Ctrl Pts',(7.09999888117586,1.32186630199077,0.628584136488803));
#9972=CARTESIAN_POINT('Ctrl Pts',(7.09999868987568,1.32059900146923,0.632813078704371));
#9973=CARTESIAN_POINT('Ctrl Pts',(7.09999860640034,1.3190551184949,0.636963663611311));
#9974=CARTESIAN_POINT('Ctrl Pts',(7.09999865766138,1.31724253497577,0.641005923298765));
#9975=CARTESIAN_POINT('Ctrl Pts',(7.0999987494091,1.31399834762864,0.648240816253195));
#9976=CARTESIAN_POINT('Ctrl Pts',(7.09999933613984,1.30993159792479,0.655050690394837));
#9977=CARTESIAN_POINT('Ctrl Pts',(7.09999956222935,1.30510592187917,0.661272231165006));
#9978=CARTESIAN_POINT('Ctrl Pts',(7.09999960444598,1.30420484616769,0.662433950108221));
#9979=CARTESIAN_POINT('Ctrl Pts',(7.09999963060969,1.30327718139331,0.663575086117144));
#9980=CARTESIAN_POINT('Ctrl Pts',(7.09999963056866,1.30232317316131,0.664694459428815));
#9981=CARTESIAN_POINT('Ctrl Pts',(7.09999963048683,1.30042028596585,0.666927187690779));
#9982=CARTESIAN_POINT('Ctrl Pts',(7.09999952705857,1.29841262431024,0.669073382394206));
#9983=CARTESIAN_POINT('Ctrl Pts',(7.09999938633452,1.29630755303174,0.671129253595323));
#9984=CARTESIAN_POINT('Ctrl Pts',(7.09999900634735,1.29062337821964,0.676680576924663));
#9985=CARTESIAN_POINT('Ctrl Pts',(7.09999841760642,1.2842958957007,0.681513596217188));
#9986=CARTESIAN_POINT('Ctrl Pts',(7.0999982224057,1.2774887935492,0.68557385059291));
#9987=CARTESIAN_POINT('Ctrl Pts',(7.09999809840912,1.27316474526651,0.688153029745784));
#9988=CARTESIAN_POINT('Ctrl Pts',(7.09999810738417,1.26864620899217,0.690419707112974));
#9989=CARTESIAN_POINT('Ctrl Pts',(7.09999825155258,1.26396949224645,0.69235064530212));
#9990=CARTESIAN_POINT('Ctrl Pts',(7.09999847710269,1.25665281355793,0.695371579659609));
#9991=CARTESIAN_POINT('Ctrl Pts',(7.09999903441007,1.2490339950321,0.697538299034574));
#9992=CARTESIAN_POINT('Ctrl Pts',(7.09999948258254,1.24125996729125,0.698781081437474));
#9993=CARTESIAN_POINT('Ctrl Pts',(7.09999977198436,1.23623998534067,0.699583592753232));
#9994=CARTESIAN_POINT('Ctrl Pts',(7.1,1.23115469319345,0.7));
#9995=CARTESIAN_POINT('Ctrl Pts',(7.1,1.22604182196307,0.7));
#9996=CARTESIAN_POINT('Ctrl Pts',(7.1,1.35793097395724,0.));
#9997=CARTESIAN_POINT('Ctrl Pts',(7.1,1.35259441576718,0.100972845781549));
#9998=CARTESIAN_POINT('Ctrl Pts',(7.1,1.34725763161617,0.201946637598055));
#9999=CARTESIAN_POINT('Ctrl Pts',(7.1,1.33659371676552,0.403704849408333));
#10000=CARTESIAN_POINT('Ctrl Pts',(7.0999999994629,1.33126648576411,0.504491180117376));
#10001=CARTESIAN_POINT('Ctrl Pts',(7.0999999994629,1.32593912634735,0.605276549957215));
#10002=CARTESIAN_POINT('Ctrl Pts',(7.11011156210589,-1.35766432821499,-9.27062925672982E-5));
#10003=CARTESIAN_POINT('Ctrl Pts',(7.10674110347764,-1.34708925835705,0.201697046690488));
#10004=CARTESIAN_POINT('Ctrl Pts',(7.10337058314201,-1.33651419103807,0.403486798779133));
#10005=CARTESIAN_POINT('Ctrl Pts',(7.09999999999996,-1.32593912631822,0.605276549958221));
#10006=CARTESIAN_POINT('Ctrl Pts',(5.9694837631095,-1.38835096090528,2.80675674898241E-6));
#10007=CARTESIAN_POINT('Ctrl Pts',(5.96835662351021,-1.37777563343505,0.201792740207853));
#10008=CARTESIAN_POINT('Ctrl Pts',(5.96722945517891,-1.3672003004237,0.40358267322573));
#10009=CARTESIAN_POINT('Ctrl Pts',(5.96610224583462,-1.35662497356325,0.605372606931572));
#10010=CARTESIAN_POINT('Ctrl Pts',(4.8294200007394,-1.39866452387306,3.01102374082134E-5));
#10011=CARTESIAN_POINT('Ctrl Pts',(4.83053730380309,-1.38808904115766,0.201820093264151));
#10012=CARTESIAN_POINT('Ctrl Pts',(4.83165461298617,-1.3775135517806,0.403610075973038));
#10013=CARTESIAN_POINT('Ctrl Pts',(4.83277191472125,-1.36693806692183,0.605400059795761));
#10014=CARTESIAN_POINT('Ctrl Pts',(3.68991216363982,-1.37907703205181,-6.2684699445455E-5));
#10015=CARTESIAN_POINT('Ctrl Pts',(3.69327498756969,-1.36850179198701,0.201727122618256));
#10016=CARTESIAN_POINT('Ctrl Pts',(3.69663785098144,-1.3579265529724,0.403516929334346));
#10017=CARTESIAN_POINT('Ctrl Pts',(3.70000075457889,-1.34735131503281,0.605306735438421));
#10018=CARTESIAN_POINT('Ctrl Pts',(3.69999999992215,-1.34735368792773,0.6052614572053));
#10019=CARTESIAN_POINT('Ctrl Pts',(4.83355316856959,-1.366961322855,0.605214762857233));
#10020=CARTESIAN_POINT('Ctrl Pts',(5.96724522208681,-1.35660163688233,0.605228569880684));
#10021=CARTESIAN_POINT('Ctrl Pts',(7.09999999927392,-1.32593912632169,0.605276549957417));
#10022=CARTESIAN_POINT('Ctrl Pts',(7.1,-1.22604182196307,0.7));
#10023=CARTESIAN_POINT('Ctrl Pts',(5.96696284938742,-1.25674179781664,0.7));
#10024=CARTESIAN_POINT('Ctrl Pts',(4.83327074934872,-1.26710800714677,0.7));
#10025=CARTESIAN_POINT('Ctrl Pts',(3.7,-1.24747724070879,0.7));
#10026=CARTESIAN_POINT('Ctrl Pts',(7.10078315634008,-1.25494559805327,0.7));
#10027=CARTESIAN_POINT('Ctrl Pts',(5.96739926106349,-1.28566432005869,0.700000343763215));
#10028=CARTESIAN_POINT('Ctrl Pts',(4.83328164159484,-1.29603890521481,0.700000334703603));
#10029=CARTESIAN_POINT('Ctrl Pts',(3.69949916377151,-1.27639017438114,0.7));
#10030=CARTESIAN_POINT('Ctrl Pts',(7.10214055788579,-1.30504291366416,0.676629771601708));
#10031=CARTESIAN_POINT('Ctrl Pts',(5.96815960929481,-1.33579288254824,0.676614006760374));
#10032=CARTESIAN_POINT('Ctrl Pts',(4.83329467960724,-1.3461818279488,0.676609489640654));
#10033=CARTESIAN_POINT('Ctrl Pts',(3.69863109538965,-1.3265031696486,0.676624836591801));
#10034=CARTESIAN_POINT('Ctrl Pts',(7.10267376869946,-1.32472200604796,0.626932241521275));
#10035=CARTESIAN_POINT('Ctrl Pts',(5.9684558952243,-1.35546668061705,0.626891484245174));
#10036=CARTESIAN_POINT('Ctrl Pts',(4.83330292199863,-1.36585610284781,0.626879766983475));
#10037=CARTESIAN_POINT('Ctrl Pts',(3.69829020046733,-1.34618280086838,0.626919440930842));
#10038=CARTESIAN_POINT('Ctrl Pts',(7.10270476209941,-1.32586587253612,0.605276664588022));
#10039=CARTESIAN_POINT('Ctrl Pts',(5.96847377630401,-1.35660073810322,0.605228567467576));
#10040=CARTESIAN_POINT('Ctrl Pts',(4.8333022084086,-1.36698748587873,0.605214711607465));
#10041=CARTESIAN_POINT('Ctrl Pts',(3.69827043673666,-1.34732374755196,0.60526152849799));
#10042=CARTESIAN_POINT('Ctrl Pts',(7.1,-1.22604182196307,0.7));
#10043=CARTESIAN_POINT('Ctrl Pts',(5.96696284938742,-1.25674179781664,0.7));
#10044=CARTESIAN_POINT('Ctrl Pts',(4.83327074934872,-1.26710800714677,0.7));
#10045=CARTESIAN_POINT('Ctrl Pts',(3.7,-1.24747724070879,0.7));
#10046=CARTESIAN_POINT('Origin',(5.4,-8.11656130105013E-18,0.7));
#10047=CARTESIAN_POINT('Ctrl Pts',(3.7,1.24747724070879,0.7));
#10048=CARTESIAN_POINT('Ctrl Pts',(4.83327074934871,1.26710800714677,0.7));
#10049=CARTESIAN_POINT('Ctrl Pts',(5.96696284938742,1.25674179781664,0.7));
#10050=CARTESIAN_POINT('Ctrl Pts',(7.1,1.22604182196307,0.7));
#10051=CARTESIAN_POINT('Ctrl Pts',(3.7,1.24747724070879,0.7));
#10052=CARTESIAN_POINT('Ctrl Pts',(4.83327074934871,1.26710800714677,0.7));
#10053=CARTESIAN_POINT('Ctrl Pts',(5.96696284938742,1.25674179781664,0.7));
#10054=CARTESIAN_POINT('Ctrl Pts',(7.1,1.22604182196307,0.7));
#10055=CARTESIAN_POINT('Ctrl Pts',(3.69949916377151,1.27639017438114,0.7));
#10056=CARTESIAN_POINT('Ctrl Pts',(4.83328164159484,1.29603890521481,0.700000334703603));
#10057=CARTESIAN_POINT('Ctrl Pts',(5.96739926106349,1.28566432005869,0.700000343763215));
#10058=CARTESIAN_POINT('Ctrl Pts',(7.10078315634008,1.25494559805327,0.7));
#10059=CARTESIAN_POINT('Ctrl Pts',(3.69863109538965,1.3265031696486,0.676624836591801));
#10060=CARTESIAN_POINT('Ctrl Pts',(4.83329467960724,1.3461818279488,0.676609489640654));
#10061=CARTESIAN_POINT('Ctrl Pts',(5.9681596092948,1.33579288254824,0.676614006760374));
#10062=CARTESIAN_POINT('Ctrl Pts',(7.10214055788579,1.30504291366416,0.676629771601707));
#10063=CARTESIAN_POINT('Ctrl Pts',(3.69829020046733,1.34618280086838,0.626919440930842));
#10064=CARTESIAN_POINT('Ctrl Pts',(4.83330292199863,1.36585610284781,0.626879766983475));
#10065=CARTESIAN_POINT('Ctrl Pts',(5.9684558952243,1.35546668061705,0.626891484245174));
#10066=CARTESIAN_POINT('Ctrl Pts',(7.10267376869946,1.32472200604796,0.626932241521275));
#10067=CARTESIAN_POINT('Ctrl Pts',(3.69827043673666,1.34732374755196,0.60526152849799));
#10068=CARTESIAN_POINT('Ctrl Pts',(4.83330220840859,1.36698748587873,0.605214711607465));
#10069=CARTESIAN_POINT('Ctrl Pts',(5.96847377630401,1.35660073810322,0.605228567467576));
#10070=CARTESIAN_POINT('Ctrl Pts',(7.10270476209941,1.32586587253612,0.605276664588022));
#10071=CARTESIAN_POINT('Ctrl Pts',(7.09999999927392,1.32593912632169,0.605276549957417));
#10072=CARTESIAN_POINT('Ctrl Pts',(5.96724522208681,1.35660163688233,0.605228569880684));
#10073=CARTESIAN_POINT('Ctrl Pts',(4.83355316856959,1.366961322855,0.605214762857233));
#10074=CARTESIAN_POINT('Ctrl Pts',(3.69999999992215,1.34735368792773,0.6052614572053));
#10075=CARTESIAN_POINT('Ctrl Pts',(3.68991216360307,1.37907703216746,-6.26869063400631E-5));
#10076=CARTESIAN_POINT('Ctrl Pts',(3.6932749875452,1.36850179206412,0.201727121146993));
#10077=CARTESIAN_POINT('Ctrl Pts',(3.69663785096921,1.35792655301095,0.403516928598715));
#10078=CARTESIAN_POINT('Ctrl Pts',(3.70000075457892,1.34735131503281,0.605306735438421));
#10079=CARTESIAN_POINT('Ctrl Pts',(4.8294200007272,1.39866452398872,3.01080305115927E-5));
#10080=CARTESIAN_POINT('Ctrl Pts',(4.83053730379496,1.38808904123477,0.201820091792887));
#10081=CARTESIAN_POINT('Ctrl Pts',(4.83165461298211,1.37751355181915,0.403610075237406));
#10082=CARTESIAN_POINT('Ctrl Pts',(4.83277191472127,1.36693806692183,0.605400059795761));
#10083=CARTESIAN_POINT('Ctrl Pts',(5.96948376312183,1.38835096102094,2.80454985295556E-6));
#10084=CARTESIAN_POINT('Ctrl Pts',(5.96835662351844,1.37777563351215,0.201792738736588));
#10085=CARTESIAN_POINT('Ctrl Pts',(5.96722945518303,1.36720030046225,0.403582672490098));
#10086=CARTESIAN_POINT('Ctrl Pts',(5.96610224583462,1.35662497356325,0.605372606931572));
#10087=CARTESIAN_POINT('Ctrl Pts',(7.11011156214274,1.35766432833065,-9.27084994613511E-5));
#10088=CARTESIAN_POINT('Ctrl Pts',(7.10674110350221,1.34708925843416,0.201697045219225));
#10089=CARTESIAN_POINT('Ctrl Pts',(7.10337058315429,1.33651419107662,0.403486798043502));
#10090=CARTESIAN_POINT('Ctrl Pts',(7.09999999999996,1.32593912631822,0.605276549958221));
#10091=CARTESIAN_POINT('Origin',(3.5,1.44777777777778,0.));
#10092=CARTESIAN_POINT('',(3.5,-1.34358136363184,0.605270327458634));
#10093=CARTESIAN_POINT('Ctrl Pts',(3.5,-1.34358136363184,0.605270327458634));
#10094=CARTESIAN_POINT('Ctrl Pts',(3.5,-1.34890136370362,0.504489156176152));
#10095=CARTESIAN_POINT('Ctrl Pts',(3.5,-1.35422123464986,0.403706701640381));
#10096=CARTESIAN_POINT('Ctrl Pts',(3.5,-1.3648706701715,0.201950780690867));
#10097=CARTESIAN_POINT('Ctrl Pts',(3.5,-1.3702003690246,0.100974756199658));
#10098=CARTESIAN_POINT('Ctrl Pts',(3.5,-1.37552980833516,0.));
#10099=CARTESIAN_POINT('',(3.5,-1.24369946473884,0.7));
#10100=CARTESIAN_POINT('Ctrl Pts',(3.49999999991873,-1.24369946470729,0.7));
#10101=CARTESIAN_POINT('Ctrl Pts',(3.49999999896975,-1.25160831520001,0.699999999810925));
#10102=CARTESIAN_POINT('Ctrl Pts',(3.50000040534574,-1.25945374057332,0.69900619751828));
#10103=CARTESIAN_POINT('Ctrl Pts',(3.50000075715473,-1.26709539726361,0.697119355224275));
#10104=CARTESIAN_POINT('Ctrl Pts',(3.5000009551612,-1.27139630362835,0.696057395447694));
#10105=CARTESIAN_POINT('Ctrl Pts',(3.50000113454144,-1.27563271975905,0.694711510656402));
#10106=CARTESIAN_POINT('Ctrl Pts',(3.50000124621709,-1.27977793997275,0.693092697679401));
#10107=CARTESIAN_POINT('Ctrl Pts',(3.50000144618968,-1.28720060051191,0.690193961644836));
#10108=CARTESIAN_POINT('Ctrl Pts',(3.50000138985083,-1.29425038514255,0.686454755369034));
#10109=CARTESIAN_POINT('Ctrl Pts',(3.5000011147959,-1.30078112659466,0.681956784255818));
#10110=CARTESIAN_POINT('Ctrl Pts',(3.50000096334461,-1.30437709646577,0.679480102439082));
#10111=CARTESIAN_POINT('Ctrl Pts',(3.50000075087427,-1.30781543681835,0.676772489296601));
#10112=CARTESIAN_POINT('Ctrl Pts',(3.50000056308077,-1.31106783354026,0.67384203444854));
#10113=CARTESIAN_POINT('Ctrl Pts',(3.50000037990614,-1.31424023611357,0.670983655445047));
#10114=CARTESIAN_POINT('Ctrl Pts',(3.50000021841608,-1.31721646102264,0.667930553458483));
#10115=CARTESIAN_POINT('Ctrl Pts',(3.50000022028926,-1.3199739184757,0.664694242102541));
#10116=CARTESIAN_POINT('Ctrl Pts',(3.50000022375892,-1.32508151834405,0.658699667848218));
#10117=CARTESIAN_POINT('Ctrl Pts',(3.50000072745304,-1.32944146850927,0.652077914129702));
#10118=CARTESIAN_POINT('Ctrl Pts',(3.50000090782832,-1.33299465793893,0.64499486611401));
#10119=CARTESIAN_POINT('Ctrl Pts',(3.50000092626355,-1.33335781125732,0.644270944003422));
#10120=CARTESIAN_POINT('Ctrl Pts',(3.50000094214549,-1.33371249714824,0.643542183465449));
#10121=CARTESIAN_POINT('Ctrl Pts',(3.5000009551778,-1.33405862411533,0.642808750463418));
#10122=CARTESIAN_POINT('Ctrl Pts',(3.50000108270827,-1.3374457225345,0.635631587173848));
#10123=CARTESIAN_POINT('Ctrl Pts',(3.5000008470667,-1.33997810357527,0.628091493562486));
#10124=CARTESIAN_POINT('Ctrl Pts',(3.50000049017339,-1.34160279315579,0.620357239364781));
#10125=CARTESIAN_POINT('Ctrl Pts',(3.50000026118253,-1.3426452308862,0.615394766232079));
#10126=CARTESIAN_POINT('Ctrl Pts',(3.5,-1.34331313055125,0.610351689051435));
#10127=CARTESIAN_POINT('Ctrl Pts',(3.5,-1.34358136363184,0.605270327458634));
#10128=CARTESIAN_POINT('',(3.5,0.723888888888889,0.7));
#10129=CARTESIAN_POINT('Ctrl Pts',(3.5,1.37552980833516,0.));
#10130=CARTESIAN_POINT('Ctrl Pts',(3.5,1.37020035376703,0.10097504527886));
#10131=CARTESIAN_POINT('Ctrl Pts',(3.5,1.36487063968137,0.201951358354439));
#10132=CARTESIAN_POINT('Ctrl Pts',(3.5,1.35422120417274,0.403707279015233));
#10133=CARTESIAN_POINT('Ctrl Pts',(3.5,1.34890134846466,0.504489444860456));
#10134=CARTESIAN_POINT('Ctrl Pts',(3.5,1.34358136363184,0.605270327458635));
#10135=CARTESIAN_POINT('Ctrl Pts',(3.50000000097418,-1.37552980835478,3.46944695195361E-18));
#10136=CARTESIAN_POINT('Ctrl Pts',(3.50374047168104,-1.36494504174376,0.201972406882836));
#10137=CARTESIAN_POINT('Ctrl Pts',(3.50748098869546,-1.35436027657305,0.403944812985359));
#10138=CARTESIAN_POINT('Ctrl Pts',(3.51122155284351,-1.34377551287676,0.605917218294091));
#10139=CARTESIAN_POINT('Ctrl Pts',(2.69119625874569,-1.35924722858667,-7.54309614812119E-5));
#10140=CARTESIAN_POINT('Ctrl Pts',(2.69653217397324,-1.34866266892899,0.20189683354744));
#10141=CARTESIAN_POINT('Ctrl Pts',(2.70186816749714,-1.3380781117335,0.403869096002786));
#10142=CARTESIAN_POINT('Ctrl Pts',(2.7072042346663,-1.32749355863083,0.605841357314298));
#10143=CARTESIAN_POINT('Ctrl Pts',(1.88267190563219,-1.32763345268679,-0.000212792412547521));
#10144=CARTESIAN_POINT('Ctrl Pts',(1.88960380459144,-1.31704931403188,0.201759213581099));
#10145=CARTESIAN_POINT('Ctrl Pts',(1.89653581411498,-1.30646518166523,0.403731216009517));
#10146=CARTESIAN_POINT('Ctrl Pts',(1.90346792975642,-1.29588105699583,0.605703215867581));
#10147=CARTESIAN_POINT('Ctrl Pts',(1.07441451989529,-1.27728918272486,-0.000429194541766893));
#10148=CARTESIAN_POINT('Ctrl Pts',(1.08294287068452,-1.26670581246828,0.201542410257184));
#10149=CARTESIAN_POINT('Ctrl Pts',(1.09147136321593,-1.25612245578053,0.403514009799157));
#10150=CARTESIAN_POINT('Ctrl Pts',(1.09999999999989,-1.24553911298205,0.605485603995245));
#10151=CARTESIAN_POINT('Ctrl Pts',(1.09999999916631,-1.24553911263844,0.605485603997431));
#10152=CARTESIAN_POINT('Ctrl Pts',(1.89930203168262,-1.29563783986497,0.605377360150118));
#10153=CARTESIAN_POINT('Ctrl Pts',(2.69958486793449,-1.32722445934619,0.605308375488923));
#10154=CARTESIAN_POINT('Ctrl Pts',(3.5,-1.34358136363184,0.605270327458634));
#10155=CARTESIAN_POINT('Ctrl Pts',(3.50204003610941,-1.24374118183538,0.7));
#10156=CARTESIAN_POINT('Ctrl Pts',(2.70080437300401,-1.2273695200909,0.7));
#10157=CARTESIAN_POINT('Ctrl Pts',(1.89984199608574,-1.1957170361627,0.7));
#10158=CARTESIAN_POINT('Ctrl Pts',(1.1,-1.14549341399196,0.7));
#10159=CARTESIAN_POINT('Ctrl Pts',(3.50144932661635,-1.27265074030048,0.7));
#10160=CARTESIAN_POINT('Ctrl Pts',(2.6998452019678,-1.25626413437997,0.699999727319846));
#10161=CARTESIAN_POINT('Ctrl Pts',(1.89847848223078,-1.22458382597074,0.70000077422621));
#10162=CARTESIAN_POINT('Ctrl Pts',(1.09819048660397,-1.17431102498992,0.7));
#10163=CARTESIAN_POINT('Ctrl Pts',(3.50042536655637,-1.322763754511,0.676632802377821));
#10164=CARTESIAN_POINT('Ctrl Pts',(2.69818680938114,-1.3063522351595,0.67664530655333));
#10165=CARTESIAN_POINT('Ctrl Pts',(1.89610976425884,-1.27462253270773,0.67666760713801));
#10166=CARTESIAN_POINT('Ctrl Pts',(1.09505363188407,-1.22426736091617,0.676703190608825));
#10167=CARTESIAN_POINT('Ctrl Pts',(3.50002334924346,-1.34243864233338,0.626926882269943));
#10168=CARTESIAN_POINT('Ctrl Pts',(2.6975332861013,-1.32603127467068,0.626959208652505));
#10169=CARTESIAN_POINT('Ctrl Pts',(1.89518106151152,-1.29430885982199,0.62701751976321));
#10170=CARTESIAN_POINT('Ctrl Pts',(1.09381704710221,-1.24396073223232,0.627109609335854));
#10171=CARTESIAN_POINT('Ctrl Pts',(3.5,-1.34358136363184,0.605270327458634));
#10172=CARTESIAN_POINT('Ctrl Pts',(2.69749615303,-1.32718177535833,0.605308474776761));
#10173=CARTESIAN_POINT('Ctrl Pts',(1.89512529323683,-1.29547288309274,0.605377720397184));
#10174=CARTESIAN_POINT('Ctrl Pts',(1.09374258853658,-1.24514653057163,0.605486452199395));
#10175=CARTESIAN_POINT('Ctrl Pts',(3.49999999991875,-1.24369946470729,0.7));
#10176=CARTESIAN_POINT('Ctrl Pts',(3.26917843083003,-1.23897560807887,0.7));
#10177=CARTESIAN_POINT('Ctrl Pts',(3.03837960179139,-1.23298334389983,0.7));
#10178=CARTESIAN_POINT('Ctrl Pts',(2.80762376541487,-1.22564400623233,0.7));
#10179=CARTESIAN_POINT('Ctrl Pts',(2.57739190516312,-1.2178709162388,0.7));
#10180=CARTESIAN_POINT('Ctrl Pts',(2.08463535466707,-1.20026407570248,0.7));
#10181=CARTESIAN_POINT('Ctrl Pts',(1.59210562457525,-1.17639367564078,0.7));
#10182=CARTESIAN_POINT('Ctrl Pts',(1.1,-1.14549341399196,0.7));
#10183=CARTESIAN_POINT('Origin',(5.4,-8.11656130105013E-18,0.7));
#10184=CARTESIAN_POINT('Ctrl Pts',(1.0744145198953,1.27728918272486,-0.000429194541767127));
#10185=CARTESIAN_POINT('Ctrl Pts',(1.08294287068452,1.26670581246828,0.201542410257184));
#10186=CARTESIAN_POINT('Ctrl Pts',(1.09147136321593,1.25612245578053,0.403514009799157));
#10187=CARTESIAN_POINT('Ctrl Pts',(1.0999999999999,1.24553911298205,0.605485603995245));
#10188=CARTESIAN_POINT('Ctrl Pts',(1.88267190563235,1.3276334526868,-0.000212792412547728));
#10189=CARTESIAN_POINT('Ctrl Pts',(1.8896038045916,1.31704931403189,0.201759213581098));
#10190=CARTESIAN_POINT('Ctrl Pts',(1.89653581411514,1.30646518166524,0.403731216009517));
#10191=CARTESIAN_POINT('Ctrl Pts',(1.90346792975658,1.29588105699584,0.605703215867581));
#10192=CARTESIAN_POINT('Ctrl Pts',(2.69119625874601,1.35924722858668,-7.54309614812134E-5));
#10193=CARTESIAN_POINT('Ctrl Pts',(2.69653217397356,1.348662668929,0.201896833547441));
#10194=CARTESIAN_POINT('Ctrl Pts',(2.70186816749745,1.33807811173351,0.403869096002786));
#10195=CARTESIAN_POINT('Ctrl Pts',(2.70720423466661,1.32749355863085,0.605841357314298));
#10196=CARTESIAN_POINT('Ctrl Pts',(3.50000000097466,1.37552980835479,-3.81639164714898E-17));
#10197=CARTESIAN_POINT('Ctrl Pts',(3.50374047168151,1.36494504174377,0.201972406882836));
#10198=CARTESIAN_POINT('Ctrl Pts',(3.50748098869594,1.35436027657306,0.403944812985359));
#10199=CARTESIAN_POINT('Ctrl Pts',(3.51122155284398,1.34377551287677,0.605917218294091));
#10200=CARTESIAN_POINT('Origin',(0.9,1.34328341716202,0.));
#10201=CARTESIAN_POINT('',(0.9,-1.23261418131727,0.605513513251856));
#10202=CARTESIAN_POINT('Ctrl Pts',(0.9,-1.23261418131727,0.605513513251856));
#10203=CARTESIAN_POINT('Ctrl Pts',(0.9,-1.23820195798151,0.504544236118289));
#10204=CARTESIAN_POINT('Ctrl Pts',(0.9,-1.24378834611607,0.403573587101897));
#10205=CARTESIAN_POINT('Ctrl Pts',(0.9,-1.25495246062481,0.201736610752668));
#10206=CARTESIAN_POINT('Ctrl Pts',(0.9,-1.26053033259331,0.100867703930409));
#10207=CARTESIAN_POINT('Ctrl Pts',(0.9,-1.266106713614,0.));
#10208=CARTESIAN_POINT('',(0.9,-1.13254484134404,0.7));
#10209=CARTESIAN_POINT('Ctrl Pts',(0.899999999937205,-1.13254484130906,
0.7));
#10210=CARTESIAN_POINT('Ctrl Pts',(0.899999996287105,-1.14047016437301,
0.699999998205918));
#10211=CARTESIAN_POINT('Ctrl Pts',(0.900001280561548,-1.14833327216777,
0.699006663725481));
#10212=CARTESIAN_POINT('Ctrl Pts',(0.900002371513522,-1.15599299513142,
0.697119896446058));
#10213=CARTESIAN_POINT('Ctrl Pts',(0.900002982478546,-1.16028266409831,
0.696063251566776));
#10214=CARTESIAN_POINT('Ctrl Pts',(0.900003528700818,-1.16450859688491,
0.694725368779139));
#10215=CARTESIAN_POINT('Ctrl Pts',(0.900003857331964,-1.16864431737637,
0.693116947675672));
#10216=CARTESIAN_POINT('Ctrl Pts',(0.900004447924614,-1.17607674172948,
0.690226407030055));
#10217=CARTESIAN_POINT('Ctrl Pts',(0.900004211500339,-1.18313828052408,
0.686496282267003));
#10218=CARTESIAN_POINT('Ctrl Pts',(0.900003280035406,-1.18968205680082,
0.682006679400108));
#10219=CARTESIAN_POINT('Ctrl Pts',(0.900002768383153,-1.19327654302499,
0.679540547464272));
#10220=CARTESIAN_POINT('Ctrl Pts',(0.900002064672634,-1.19671453445753,
0.676844382327844));
#10221=CARTESIAN_POINT('Ctrl Pts',(0.900001450170085,-1.19996775918788,
0.673925988054463));
#10222=CARTESIAN_POINT('Ctrl Pts',(0.900000850201302,-1.20314404102283,
0.67107661751105));
#10223=CARTESIAN_POINT('Ctrl Pts',(0.900000329673364,-1.20612495630093,
0.668032594545539));
#10224=CARTESIAN_POINT('Ctrl Pts',(0.900000346081477,-1.20888784276431,
0.664805176146368));
#10225=CARTESIAN_POINT('Ctrl Pts',(0.900000376514472,-1.21401231436848,
0.658819112599938));
#10226=CARTESIAN_POINT('Ctrl Pts',(0.900002057232535,-1.21838968018573,
0.652203523053766));
#10227=CARTESIAN_POINT('Ctrl Pts',(0.900002698394847,-1.22195969054856,
0.645123732731769));
#10228=CARTESIAN_POINT('Ctrl Pts',(0.900002763240662,-1.22232075393107,
0.644407697543824));
#10229=CARTESIAN_POINT('Ctrl Pts',(0.90000282009371,-1.22267351953901,0.643686895083047));
#10230=CARTESIAN_POINT('Ctrl Pts',(0.900002868017411,-1.22301789747605,
0.642961485862499));
#10231=CARTESIAN_POINT('Ctrl Pts',(0.900003341628975,-1.22642125256928,
0.635792544708285));
#10232=CARTESIAN_POINT('Ctrl Pts',(0.900002645022176,-1.22896979279554,
0.628258742918086));
#10233=CARTESIAN_POINT('Ctrl Pts',(0.900001532827652,-1.23061007098772,
0.6205286650049));
#10234=CARTESIAN_POINT('Ctrl Pts',(0.900000822323555,-1.23165793118585,
0.61559045329652));
#10235=CARTESIAN_POINT('Ctrl Pts',(0.900000000000001,-1.23233426661673,
0.610571479357261));
#10236=CARTESIAN_POINT('Ctrl Pts',(0.900000000000001,-1.23261418131727,
0.605513513251856));
#10237=CARTESIAN_POINT('',(0.9,1.13254484134404,0.7));
#10238=CARTESIAN_POINT('',(0.9,0.671641708581009,0.7));
#10239=CARTESIAN_POINT('',(0.9,1.23261418131727,0.605513513251856));
#10240=CARTESIAN_POINT('Ctrl Pts',(0.9,1.23261418131727,0.605513513251856));
#10241=CARTESIAN_POINT('Ctrl Pts',(0.9,1.23217633603244,0.613425232807268));
#10242=CARTESIAN_POINT('Ctrl Pts',(0.900001832787994,1.23077105609892,0.621244170085157));
#10243=CARTESIAN_POINT('Ctrl Pts',(0.900002580745575,1.22848219166492,0.628809599741497));
#10244=CARTESIAN_POINT('Ctrl Pts',(0.900002993068559,1.22722042035689,0.632980157827643));
#10245=CARTESIAN_POINT('Ctrl Pts',(0.90000314174678,1.22568915198244,0.637073706995481));
#10246=CARTESIAN_POINT('Ctrl Pts',(0.900002971484041,1.2238959908032,0.641061424759933));
#10247=CARTESIAN_POINT('Ctrl Pts',(0.900002662567364,1.22064256379503,0.648296551655426));
#10248=CARTESIAN_POINT('Ctrl Pts',(0.900001146653719,1.21656554418039,0.655104870690721));
#10249=CARTESIAN_POINT('Ctrl Pts',(0.900000540233788,1.21172928299109,0.66132323772617));
#10250=CARTESIAN_POINT('Ctrl Pts',(0.900000424918953,1.21080963534652,0.66250570210793));
#10251=CARTESIAN_POINT('Ctrl Pts',(0.900000351402035,1.20986240082127,0.663666762843393));
#10252=CARTESIAN_POINT('Ctrl Pts',(0.900000346234225,1.20888784277449,0.664805176146358));
#10253=CARTESIAN_POINT('Ctrl Pts',(0.900000336405833,1.20703438079614,0.666970266034709));
#10254=CARTESIAN_POINT('Ctrl Pts',(0.900000571869483,1.20508211779724,0.669053482241208));
#10255=CARTESIAN_POINT('Ctrl Pts',(0.900000903580486,1.20303784749416,0.671051418948595));
#10256=CARTESIAN_POINT('Ctrl Pts',(0.900001825932764,1.19735357006848,0.676606861644505));
#10257=CARTESIAN_POINT('Ctrl Pts',(0.900003332967427,1.19102482074992,0.681443262092019));
#10258=CARTESIAN_POINT('Ctrl Pts',(0.900003895332687,1.18421635668109,0.685507797106414));
#10259=CARTESIAN_POINT('Ctrl Pts',(0.900004254598985,1.17986677848026,0.688104419886002));
#10260=CARTESIAN_POINT('Ctrl Pts',(0.9000042929279,1.17532044218795,0.69038534615497));
#10261=CARTESIAN_POINT('Ctrl Pts',(0.900003997675654,1.17061445353731,0.692327416690341));
#10262=CARTESIAN_POINT('Ctrl Pts',(0.900003537640084,1.16328200409216,0.695353376818313));
#10263=CARTESIAN_POINT('Ctrl Pts',(0.900002259964378,1.15564663185935,0.697524398440697));
#10264=CARTESIAN_POINT('Ctrl Pts',(0.900001215101098,1.14785635641255,0.698771715080855));
#10265=CARTESIAN_POINT('Ctrl Pts',(0.900000537649455,1.14280542295857,0.699580430175527));
#10266=CARTESIAN_POINT('Ctrl Pts',(0.899999997568109,1.13768876957788,0.699999998835552));
#10267=CARTESIAN_POINT('Ctrl Pts',(0.899999999937205,1.13254484130906,0.7));
#10268=CARTESIAN_POINT('Ctrl Pts',(0.9,1.266106713614,0.));
#10269=CARTESIAN_POINT('Ctrl Pts',(0.9,1.26053025554556,0.100869097599589));
#10270=CARTESIAN_POINT('Ctrl Pts',(0.9,1.25495230648558,0.201739398169819));
#10271=CARTESIAN_POINT('Ctrl Pts',(0.9,1.24378819189631,0.403576374532447));
#10272=CARTESIAN_POINT('Ctrl Pts',(0.9,1.23820188085298,0.504545629805417));
#10273=CARTESIAN_POINT('Ctrl Pts',(0.9,1.23261418131727,0.605513513251856));
#10274=CARTESIAN_POINT('Ctrl Pts',(0.900000000000002,-1.266106713614,-8.15320033709099E-17));
#10275=CARTESIAN_POINT('Ctrl Pts',(0.908871090277923,-1.25552568177643,
0.201930159665972));
#10276=CARTESIAN_POINT('Ctrl Pts',(0.917742329685194,-1.24494466498547,
0.403860313587921));
#10277=CARTESIAN_POINT('Ctrl Pts',(0.926613720860141,-1.23436366359623,
0.605790461668883));
#10278=CARTESIAN_POINT('Ctrl Pts',(0.697441255022372,-1.25280938151844,
-5.71013218131409E-5));
#10279=CARTESIAN_POINT('Ctrl Pts',(0.706712389899261,-1.24222855501813,
0.201872952723963));
#10280=CARTESIAN_POINT('Ctrl Pts',(0.71598368260269,-1.23164774534186,0.403803000441224));
#10281=CARTESIAN_POINT('Ctrl Pts',(0.725255135891715,-1.22106695288555,
0.605733041729342));
#10282=CARTESIAN_POINT('Ctrl Pts',(0.494899146035781,-1.23832021354117,
-0.000119230777047918));
#10283=CARTESIAN_POINT('Ctrl Pts',(0.504570354086872,-1.2277396148863,0.201810708652083));
#10284=CARTESIAN_POINT('Ctrl Pts',(0.514241728780064,-1.21715903502506,
0.403740641123913));
#10285=CARTESIAN_POINT('Ctrl Pts',(0.523913273026478,-1.20657847439907,
0.605670566527588));
#10286=CARTESIAN_POINT('Ctrl Pts',(0.292373353339556,-1.22258574808743,
-0.000186633859775947));
#10287=CARTESIAN_POINT('Ctrl Pts',(0.302444661323169,-1.21200540195431,
0.201743181663441));
#10288=CARTESIAN_POINT('Ctrl Pts',(0.312516144861689,-1.20142507679253,
0.403672989556125));
#10289=CARTESIAN_POINT('Ctrl Pts',(0.322587807049886,-1.190844773096,0.605602789690272));
#10290=CARTESIAN_POINT('',(0.32407846024449,-1.19096124572524,0.605603291426262));
#10291=CARTESIAN_POINT('Ctrl Pts',(0.292382661757373,-1.22257596919059,
-1.26634813746307E-16));
#10292=CARTESIAN_POINT('Ctrl Pts',(0.302948004341657,-1.21203750712027,
0.201867748891544));
#10293=CARTESIAN_POINT('Ctrl Pts',(0.313513270922098,-1.20149926476964,
0.403735512620674));
#10294=CARTESIAN_POINT('Ctrl Pts',(0.324078460244491,-1.19096124572524,
0.605603291426262));
#10295=CARTESIAN_POINT('Ctrl Pts',(0.324078460244487,-1.19096124572524,
0.605603291426262));
#10296=CARTESIAN_POINT('Ctrl Pts',(0.515976798438381,-1.20595780001216,
0.605571001180369));
#10297=CARTESIAN_POINT('Ctrl Pts',(0.707956283694857,-1.21982772882273,
0.605541108414459));
#10298=CARTESIAN_POINT('Ctrl Pts',(0.900000000000001,-1.23261418131727,
0.605513513251856));
#10299=CARTESIAN_POINT('Ctrl Pts',(0.906632491847682,-1.13298681949577,
0.7));
#10300=CARTESIAN_POINT('Ctrl Pts',(0.714963137593258,-1.12022681655782,
0.7));
#10301=CARTESIAN_POINT('Ctrl Pts',(0.52336552158394,-1.10638609587519,0.7));
#10302=CARTESIAN_POINT('Ctrl Pts',(0.331856371369197,-1.09142177001972,
0.7));
#10303=CARTESIAN_POINT('Ctrl Pts',(0.904714827274509,-1.16179226195561,
0.7));
#10304=CARTESIAN_POINT('Ctrl Pts',(0.712937153454425,-1.14901967286075,
0.69999980360337));
#10305=CARTESIAN_POINT('Ctrl Pts',(0.521230340369869,-1.13516557394852,
0.700000229443053));
#10306=CARTESIAN_POINT('Ctrl Pts',(0.329608751265076,-1.12018616744754,
0.7));
#10307=CARTESIAN_POINT('Ctrl Pts',(0.901389714107723,-1.21173913866089,
0.676722045797292));
#10308=CARTESIAN_POINT('Ctrl Pts',(0.709425477581998,-1.19894546296063,
0.676731074746188));
#10309=CARTESIAN_POINT('Ctrl Pts',(0.517526696841433,-1.18506766126723,
0.67674067107047));
#10310=CARTESIAN_POINT('Ctrl Pts',(0.325711429829026,-1.17006296935233,
0.676751229163451));
#10311=CARTESIAN_POINT('Ctrl Pts',(0.900079298017777,-1.23142303740181,
0.627132481749528));
#10312=CARTESIAN_POINT('Ctrl Pts',(0.708040181852795,-1.21863106773591,
0.627155851652593));
#10313=CARTESIAN_POINT('Ctrl Pts',(0.516066269599777,-1.20475540724405,
0.627181012790208));
#10314=CARTESIAN_POINT('Ctrl Pts',(0.324172915772929,-1.18975243096407,
0.627208352638976));
#10315=CARTESIAN_POINT('Ctrl Pts',(0.900000000000001,-1.23261418131727,
0.605513513251856));
#10316=CARTESIAN_POINT('Ctrl Pts',(0.707956283694857,-1.21982772882273,
0.605541108414459));
#10317=CARTESIAN_POINT('Ctrl Pts',(0.515976798438381,-1.20595780001216,
0.605571001180369));
#10318=CARTESIAN_POINT('Ctrl Pts',(0.324078460244487,-1.19096124572524,
0.605603291426262));
#10319=CARTESIAN_POINT('',(0.3318563713692,-1.09142177001972,0.7));
#10320=CARTESIAN_POINT('Origin',(0.3318563713692,-1.09142177001972,0.6));
#10321=CARTESIAN_POINT('Ctrl Pts',(0.899999999937167,-1.13254484130906,
0.7));
#10322=CARTESIAN_POINT('Ctrl Pts',(0.710543123935439,-1.11990737114256,
0.7));
#10323=CARTESIAN_POINT('Ctrl Pts',(0.521156529292483,-1.10621348751457,
0.7));
#10324=CARTESIAN_POINT('Ctrl Pts',(0.331856371369197,-1.09142177001972,
0.7));
#10325=CARTESIAN_POINT('Origin',(5.4,-8.11656130105013E-18,0.7));
#10326=CARTESIAN_POINT('',(0.3318563713692,1.09142177001972,0.7));
#10327=CARTESIAN_POINT('',(0.3318563713692,-0.7,0.7));
#10328=CARTESIAN_POINT('Ctrl Pts',(0.3318563713692,1.09142177001972,0.7));
#10329=CARTESIAN_POINT('Ctrl Pts',(0.521156529292483,1.10621348751457,0.7));
#10330=CARTESIAN_POINT('Ctrl Pts',(0.710543123935438,1.11990737114256,0.7));
#10331=CARTESIAN_POINT('Ctrl Pts',(0.899999999937165,1.13254484130906,0.7));
#10332=CARTESIAN_POINT('Ctrl Pts',(0.292373353339556,1.22258574808743,-0.000186633859776018));
#10333=CARTESIAN_POINT('Ctrl Pts',(0.30244466132317,1.21200540195431,0.20174318166344));
#10334=CARTESIAN_POINT('Ctrl Pts',(0.31251614486169,1.20142507679253,0.403672989556124));
#10335=CARTESIAN_POINT('Ctrl Pts',(0.322587807049886,1.190844773096,0.605602789690271));
#10336=CARTESIAN_POINT('Ctrl Pts',(0.494899146035781,1.23832021354117,-0.000119230777047989));
#10337=CARTESIAN_POINT('Ctrl Pts',(0.504570354086872,1.2277396148863,0.201810708652083));
#10338=CARTESIAN_POINT('Ctrl Pts',(0.514241728780064,1.21715903502506,0.403740641123914));
#10339=CARTESIAN_POINT('Ctrl Pts',(0.523913273026478,1.20657847439907,0.605670566527587));
#10340=CARTESIAN_POINT('Ctrl Pts',(0.697441255022371,1.25280938151844,-5.71013218130602E-5));
#10341=CARTESIAN_POINT('Ctrl Pts',(0.70671238989926,1.24222855501813,0.201872952723963));
#10342=CARTESIAN_POINT('Ctrl Pts',(0.715983682602689,1.23164774534186,0.403803000441224));
#10343=CARTESIAN_POINT('Ctrl Pts',(0.725255135891714,1.22106695288555,0.605733041729342));
#10344=CARTESIAN_POINT('Ctrl Pts',(0.9,1.266106713614,1.73472347597681E-18));
#10345=CARTESIAN_POINT('Ctrl Pts',(0.908871090277921,1.25552568177643,0.201930159665973));
#10346=CARTESIAN_POINT('Ctrl Pts',(0.917742329685192,1.24494466498547,0.403860313587921));
#10347=CARTESIAN_POINT('Ctrl Pts',(0.92661372086014,1.23436366359623,0.605790461668883));
#10348=CARTESIAN_POINT('',(0.32407846024449,1.19096124572524,0.605603291426262));
#10349=CARTESIAN_POINT('Ctrl Pts',(0.9,1.23261418131727,0.605513513251856));
#10350=CARTESIAN_POINT('Ctrl Pts',(0.707956283694857,1.21982772882273,0.605541108414459));
#10351=CARTESIAN_POINT('Ctrl Pts',(0.515976798438382,1.20595780001216,0.60557100118037));
#10352=CARTESIAN_POINT('Ctrl Pts',(0.32407846024449,1.19096124572524,0.605603291426262));
#10353=CARTESIAN_POINT('Ctrl Pts',(0.324078460244491,1.19096124572524,0.605603291426262));
#10354=CARTESIAN_POINT('Ctrl Pts',(0.313513270922098,1.20149926476964,0.403735512620674));
#10355=CARTESIAN_POINT('Ctrl Pts',(0.302948004341658,1.21203750712026,0.201867748891544));
#10356=CARTESIAN_POINT('Ctrl Pts',(0.292382661757373,1.22257596919059,3.4477629085039E-17));
#10357=CARTESIAN_POINT('Ctrl Pts',(0.3318563713692,1.09142177001972,0.7));
#10358=CARTESIAN_POINT('Ctrl Pts',(0.523365521583941,1.10638609587519,0.7));
#10359=CARTESIAN_POINT('Ctrl Pts',(0.714963137593258,1.12022681655782,0.7));
#10360=CARTESIAN_POINT('Ctrl Pts',(0.906632491847681,1.13298681949577,0.7));
#10361=CARTESIAN_POINT('Ctrl Pts',(0.329608751265078,1.12018616744754,0.7));
#10362=CARTESIAN_POINT('Ctrl Pts',(0.52123034036987,1.13516557394852,0.700000229443053));
#10363=CARTESIAN_POINT('Ctrl Pts',(0.712937153454426,1.14901967286075,0.699999803603371));
#10364=CARTESIAN_POINT('Ctrl Pts',(0.904714827274509,1.16179226195561,0.700000000000001));
#10365=CARTESIAN_POINT('Ctrl Pts',(0.325711429829028,1.17006296935233,0.676751229163452));
#10366=CARTESIAN_POINT('Ctrl Pts',(0.517526696841433,1.18506766126723,0.67674067107047));
#10367=CARTESIAN_POINT('Ctrl Pts',(0.709425477581997,1.19894546296063,0.676731074746189));
#10368=CARTESIAN_POINT('Ctrl Pts',(0.901389714107722,1.21173913866089,0.676722045797292));
#10369=CARTESIAN_POINT('Ctrl Pts',(0.324172915772932,1.18975243096407,0.627208352638976));
#10370=CARTESIAN_POINT('Ctrl Pts',(0.516066269599778,1.20475540724405,0.627181012790208));
#10371=CARTESIAN_POINT('Ctrl Pts',(0.708040181852794,1.21863106773591,0.627155851652593));
#10372=CARTESIAN_POINT('Ctrl Pts',(0.900079298017776,1.23142303740181,0.627132481749528));
#10373=CARTESIAN_POINT('Ctrl Pts',(0.32407846024449,1.19096124572524,0.605603291426262));
#10374=CARTESIAN_POINT('Ctrl Pts',(0.515976798438382,1.20595780001216,0.60557100118037));
#10375=CARTESIAN_POINT('Ctrl Pts',(0.707956283694857,1.21982772882273,0.605541108414459));
#10376=CARTESIAN_POINT('Ctrl Pts',(0.9,1.23261418131727,0.605513513251856));
#10377=CARTESIAN_POINT('Origin',(0.331856371369202,1.09142177001972,0.6));
#10378=CARTESIAN_POINT('Origin',(0.331856371369202,1.09142177001972,0.6));
#10379=CARTESIAN_POINT('Origin',(0.331856371369201,1.09142177001972,0.6));
#10380=CARTESIAN_POINT('Origin',(0.331856371369202,1.09142177001972,0.6));
#10381=CARTESIAN_POINT('Origin',(10.4681436286308,1.08420482079361,0.6));
#10382=CARTESIAN_POINT('Origin',(10.4681436276939,1.08420482084454,0.6));
#10383=CARTESIAN_POINT('',(10.5680065821063,1.08420482079361,0.605233595624295));
#10384=CARTESIAN_POINT('Origin',(10.4681436286308,1.08420482079361,0.6));
#10385=CARTESIAN_POINT('Origin',(10.4681436286308,1.08420482079361,0.6));
#10386=CARTESIAN_POINT('Origin',(0.3318563713692,-1.09142177001972,0.6));
#10387=CARTESIAN_POINT('Origin',(0.331856371369201,-1.09142177001972,0.6));
#10388=CARTESIAN_POINT('Origin',(0.3318563713692,-1.09142177001972,0.6));
#10389=CARTESIAN_POINT('Origin',(0.3318563713692,-0.7,0.6));
#10390=CARTESIAN_POINT('Ctrl Pts',(0.2922895713475,-1.22266882276207,-0.00177864096060679));
#10391=CARTESIAN_POINT('Ctrl Pts',(0.302885944515497,-1.21209940820877,
0.200681988163859));
#10392=CARTESIAN_POINT('Ctrl Pts',(0.313482241236256,-1.20153021465708,
0.403142632212487));
#10393=CARTESIAN_POINT('Ctrl Pts',(0.324078460244491,-1.19096124572524,
0.605603291426262));
#10394=CARTESIAN_POINT('Ctrl Pts',(0.264022491930188,-1.22039553779506,
-0.000415890128406236));
#10395=CARTESIAN_POINT('Ctrl Pts',(0.274621881512248,-1.20982222712748,
0.202044379074236));
#10396=CARTESIAN_POINT('Ctrl Pts',(0.285221154833576,-1.19924944554801,
0.404504681968985));
#10397=CARTESIAN_POINT('Ctrl Pts',(0.29582042516239,-1.18867654001483,0.606964977361795));
#10398=CARTESIAN_POINT('Ctrl Pts',(0.216712469170969,-1.1940874043406,0.000690255297866666));
#10399=CARTESIAN_POINT('Ctrl Pts',(0.227319688237882,-1.18351239299796,
0.203150045648192));
#10400=CARTESIAN_POINT('Ctrl Pts',(0.237926932441998,-1.17293746916702,
0.405609838636422));
#10401=CARTESIAN_POINT('Ctrl Pts',(0.248534117816369,-1.1623628476683,0.608069650238703));
#10402=CARTESIAN_POINT('Ctrl Pts',(0.200219987929043,-1.14439035743082,
-0.00103956457010847));
#10403=CARTESIAN_POINT('Ctrl Pts',(0.210830491339948,-1.13382006821851,
0.201420337884579));
#10404=CARTESIAN_POINT('Ctrl Pts',(0.221440906577676,-1.12324995278282,
0.403880253819325));
#10405=CARTESIAN_POINT('Ctrl Pts',(0.232051411471599,-1.11268010558856,
0.606340179010355));
#10406=CARTESIAN_POINT('Ctrl Pts',(0.200161975173303,-1.12312592850316,
-0.00214651389202307));
#10407=CARTESIAN_POINT('Ctrl Pts',(0.210772455448684,-1.11255764422181,
0.200313510564959));
#10408=CARTESIAN_POINT('Ctrl Pts',(0.221382936352032,-1.1019895901204,0.402773547004277));
#10409=CARTESIAN_POINT('Ctrl Pts',(0.231993417893744,-1.09142177001972,
0.605233595624295));
#10410=CARTESIAN_POINT('Origin',(10.4681436286308,-1.08420482109828,0.6));
#10411=CARTESIAN_POINT('',(10.5680065821063,-1.08420482079361,0.605233595624295));
#10412=CARTESIAN_POINT('Origin',(10.4681436286308,-1.08420482099672,0.600000000000001));
#10413=CARTESIAN_POINT('Origin',(10.4681436286308,-1.08420482109828,0.6));
#10414=CARTESIAN_POINT('Origin',(10.4681436286308,0.7,0.6));
#10415=CARTESIAN_POINT('',(10.5680065821063,0.7,0.605233595624295));
#10416=CARTESIAN_POINT('Ctrl Pts',(10.599839982685,-1.11594741464673,-0.00218387205330164));
#10417=CARTESIAN_POINT('Ctrl Pts',(10.5892288496247,-1.10536637943871,0.200288608282177));
#10418=CARTESIAN_POINT('Ctrl Pts',(10.5786177161011,-1.0947855138519,0.402761097457634));
#10419=CARTESIAN_POINT('Ctrl Pts',(10.5680065821063,-1.08420482079362,0.605233595624295));
#10420=CARTESIAN_POINT('Ctrl Pts',(10.5997613205547,-1.14474784499259,-0.000682909193257743));
#10421=CARTESIAN_POINT('Ctrl Pts',(10.5891501209488,-1.13416481604349,0.201789447273867));
#10422=CARTESIAN_POINT('Ctrl Pts',(10.5785391399155,-1.12358205581644,0.404261829287571));
#10423=CARTESIAN_POINT('Ctrl Pts',(10.5679279386544,-1.11299934606825,0.606734202078189));
#10424=CARTESIAN_POINT('Ctrl Pts',(10.5764119435127,-1.19466846760808,0.000702210001053139));
#10425=CARTESIAN_POINT('Ctrl Pts',(10.5658041809617,-1.18408222297768,0.203174550667819));
#10426=CARTESIAN_POINT('Ctrl Pts',(10.5551963844732,-1.17349608774572,0.405646894856767));
#10427=CARTESIAN_POINT('Ctrl Pts',(10.544588659013,-1.16291012508165,0.608119251464957));
#10428=CARTESIAN_POINT('Ctrl Pts',(10.5269342003857,-1.21442651155969,-0.000858270497959616));
#10429=CARTESIAN_POINT('Ctrl Pts',(10.5163317654776,-1.20384274018949,0.201614467507756));
#10430=CARTESIAN_POINT('Ctrl Pts',(10.5057293269973,-1.1932591813998,0.404087216090532));
#10431=CARTESIAN_POINT('Ctrl Pts',(10.4951269905998,-1.18267571840064,0.606559974437339));
#10432=CARTESIAN_POINT('Ctrl Pts',(10.5053655128635,-1.21565094114741,-0.0019246498908503));
#10433=CARTESIAN_POINT('Ctrl Pts',(10.4947646468921,-1.20506932615592,0.200548282383137));
#10434=CARTESIAN_POINT('Ctrl Pts',(10.4841638390504,-1.19448787589602,0.403021225840181));
#10435=CARTESIAN_POINT('Ctrl Pts',(10.4735630903435,-1.18390659316268,0.605494180667945));
#10436=CARTESIAN_POINT('Ctrl Pts',(10.5997255308004,-1.11583328740478,1.02782365951626E-16));
#10437=CARTESIAN_POINT('Ctrl Pts',(10.589152548365,-1.10529029582828,0.201744523047832));
#10438=CARTESIAN_POINT('Ctrl Pts',(10.5785795654695,-1.09474747266587,0.40348905487273));
#10439=CARTESIAN_POINT('Ctrl Pts',(10.5680065821063,-1.08420482079362,0.605233595624295));
#10440=CARTESIAN_POINT('Ctrl Pts',(10.5053638082297,1.21564923960921,-0.0018920919656423));
#10441=CARTESIAN_POINT('Ctrl Pts',(10.4947635104759,1.20506819181477,0.200569987667808));
#10442=CARTESIAN_POINT('Ctrl Pts',(10.4841632708454,1.19448730873444,0.403032078483127));
#10443=CARTESIAN_POINT('Ctrl Pts',(10.4735630903435,1.18390659316268,0.605494180667945));
#10444=CARTESIAN_POINT('Ctrl Pts',(10.5341220579192,1.21401666636749,-0.000470252816738081));
#10445=CARTESIAN_POINT('Ctrl Pts',(10.5235196325477,1.20343268662274,0.201991562854702));
#10446=CARTESIAN_POINT('Ctrl Pts',(10.5129172908767,1.19284910679518,0.404453403808947));
#10447=CARTESIAN_POINT('Ctrl Pts',(10.5023149573519,1.18226542681329,0.606915239027137));
#10448=CARTESIAN_POINT('Ctrl Pts',(10.5827170203615,1.18801090922716,0.000717463067903341));
#10449=CARTESIAN_POINT('Ctrl Pts',(10.5721088691741,1.17742555398174,0.203178921531494));
#10450=CARTESIAN_POINT('Ctrl Pts',(10.5615007184277,1.16684027916303,0.405640383775807));
#10451=CARTESIAN_POINT('Ctrl Pts',(10.5508925935528,1.15625520969485,0.60810185787831));
#10452=CARTESIAN_POINT('Ctrl Pts',(10.5997792798033,1.13754603572512,-0.00102559206997387));
#10453=CARTESIAN_POINT('Ctrl Pts',(10.5891686973038,1.12696411138589,0.201435946515793));
#10454=CARTESIAN_POINT('Ctrl Pts',(10.5785581831385,1.11638231376635,0.40389749513889));
#10455=CARTESIAN_POINT('Ctrl Pts',(10.5679475995174,1.10580071474959,0.606359050464716));
#10456=CARTESIAN_POINT('Ctrl Pts',(10.5998382764002,1.11594571320176,-0.00215131420076595));
#10457=CARTESIAN_POINT('Ctrl Pts',(10.5892277121014,1.10536524516024,0.200310313518148));
#10458=CARTESIAN_POINT('Ctrl Pts',(10.5786171473394,1.09478494672192,0.402771950076102));
#10459=CARTESIAN_POINT('Ctrl Pts',(10.5680065821063,1.08420482079361,0.605233595624295));
#10460=CARTESIAN_POINT('Ctrl Pts',(10.5680065821063,1.08420482079361,0.605233595624295));
#10461=CARTESIAN_POINT('Ctrl Pts',(10.5785795654695,1.09474747266587,0.40348905487273));
#10462=CARTESIAN_POINT('Ctrl Pts',(10.589152548365,1.10529029582828,0.201744523047831));
#10463=CARTESIAN_POINT('Ctrl Pts',(10.5997255308004,1.11583328740478,1.07661275727811E-16));
#10464=CARTESIAN_POINT('Ctrl Pts',(10.1947388861048,1.09885088260187,0.7));
#10465=CARTESIAN_POINT('Ctrl Pts',(10.285877616441,1.09404209584202,0.7));
#10466=CARTESIAN_POINT('Ctrl Pts',(10.3770124662346,1.0891584122264,0.7));
#10467=CARTESIAN_POINT('Ctrl Pts',(10.4681436286308,1.08420482079361,0.7));
#10468=CARTESIAN_POINT('Ctrl Pts',(10.196260416419,1.12768774893097,0.700000000000001));
#10469=CARTESIAN_POINT('Ctrl Pts',(10.2874149314686,1.12287675076168,0.699999949550842));
#10470=CARTESIAN_POINT('Ctrl Pts',(10.3785648662465,1.11799094453753,0.700000051218742));
#10471=CARTESIAN_POINT('Ctrl Pts',(10.4697107510168,1.11303515260326,0.7));
#10472=CARTESIAN_POINT('Ctrl Pts',(10.1988975981852,1.17766904563614,0.67669140632491));
#10473=CARTESIAN_POINT('Ctrl Pts',(10.2900793016129,1.17285439035486,0.676693724638983));
#10474=CARTESIAN_POINT('Ctrl Pts',(10.3812557252598,1.16796482352885,0.676696026813929));
#10475=CARTESIAN_POINT('Ctrl Pts',(10.4724269697127,1.16300539549315,0.676698381019544));
#10476=CARTESIAN_POINT('Ctrl Pts',(10.1999375452555,1.19737868557977,0.627098033786781));
#10477=CARTESIAN_POINT('Ctrl Pts',(10.2911301919381,1.19256517083271,0.627104033151799));
#10478=CARTESIAN_POINT('Ctrl Pts',(10.382317043787,1.18767684023183,0.627110048826767));
#10479=CARTESIAN_POINT('Ctrl Pts',(10.4734985149421,1.18271860027509,0.627116141711795));
#10480=CARTESIAN_POINT('Ctrl Pts',(10.1999999975038,1.19856231440453,0.605472757505366));
#10481=CARTESIAN_POINT('Ctrl Pts',(10.2911933328565,1.19375025772558,0.605479840815741));
#10482=CARTESIAN_POINT('Ctrl Pts',(10.3823809652617,1.18886335120032,0.605486986548286));
#10483=CARTESIAN_POINT('Ctrl Pts',(10.4735630903435,1.18390659316268,0.605494180667944));
#10484=CARTESIAN_POINT('Ctrl Pts',(0.200159601751749,1.12312829248604,-0.00219180147311912));
#10485=CARTESIAN_POINT('Ctrl Pts',(0.210770873167554,1.11255922017607,0.200283318842441));
#10486=CARTESIAN_POINT('Ctrl Pts',(0.221382145211419,1.10199037808008,0.402758451142111));
#10487=CARTESIAN_POINT('Ctrl Pts',(0.231993417893744,1.09142177001972,0.605233595624295));
#10488=CARTESIAN_POINT('Ctrl Pts',(0.200236952094631,1.15148086499205,-0.000715869007730825));
#10489=CARTESIAN_POINT('Ctrl Pts',(0.210848310847714,1.14090905181173,0.201759082033021));
#10490=CARTESIAN_POINT('Ctrl Pts',(0.221459381762758,1.13033759660317,0.404234066901971));
#10491=CARTESIAN_POINT('Ctrl Pts',(0.232070742664217,1.11976621744484,0.606709040139042));
#10492=CARTESIAN_POINT('Ctrl Pts',(0.222806696702742,1.20067708175657,0.000669311976984441));
#10493=CARTESIAN_POINT('Ctrl Pts',(0.233413416075889,1.19010082554658,0.203144236955742));
#10494=CARTESIAN_POINT('Ctrl Pts',(0.244020198555212,1.17952469009474,0.405619164345205));
#10495=CARTESIAN_POINT('Ctrl Pts',(0.254626870458834,1.16894881850735,0.608094110943904));
#10496=CARTESIAN_POINT('Ctrl Pts',(0.271086891015657,1.22096622390789,-0.000801865493577694));
#10497=CARTESIAN_POINT('Ctrl Pts',(0.281686280594249,1.21039315447922,0.201673594461172));
#10498=CARTESIAN_POINT('Ctrl Pts',(0.292285672737775,1.1998203699977,0.404149068703718));
#10499=CARTESIAN_POINT('Ctrl Pts',(0.302884933932915,1.18924771644243,0.606624555877912));
#10500=CARTESIAN_POINT('Ctrl Pts',(0.292287201081515,1.22267118699778,-0.00182392867695869));
#10501=CARTESIAN_POINT('Ctrl Pts',(0.302884364349574,1.21210098433295,0.200651796350731));
#10502=CARTESIAN_POINT('Ctrl Pts',(0.313481451159089,1.20153100270242,0.403127536304793));
#10503=CARTESIAN_POINT('Ctrl Pts',(0.324078460244491,1.19096124572524,0.605603291426262));
#10504=CARTESIAN_POINT('Origin',(10.6002740930491,1.4,-0.0104671912485891));
#10505=CARTESIAN_POINT('Origin',(0.331856371369202,1.09142177001972,0.6));
#10506=CARTESIAN_POINT('',(0.3318563713692,1.09142177001972,0.9));
#10507=CARTESIAN_POINT('',(0.0322675109428288,1.09142177001972,0.615700786872883));
#10508=CARTESIAN_POINT('Origin',(0.3318563713692,1.09142177001972,0.6));
#10509=CARTESIAN_POINT('',(0.308522637995069,1.39004019713626,0.616809874278785));
#10510=CARTESIAN_POINT('Origin',(0.331856371369202,1.09142177001972,0.6));
#10511=CARTESIAN_POINT('Origin',(0.331856371369201,1.09142177001972,0.6));
#10512=CARTESIAN_POINT('Origin',(10.4681436286308,1.08420482079361,0.6));
#10513=CARTESIAN_POINT('',(10.4681436286308,1.08420482109828,0.9));
#10514=CARTESIAN_POINT('',(10.4844020137689,1.3833101379008,0.616482542003833));
#10515=CARTESIAN_POINT('Origin',(10.4681436258201,1.08420482094639,0.6));
#10516=CARTESIAN_POINT('',(10.7677324890572,1.08420482079361,0.615700786872884));
#10517=CARTESIAN_POINT('Origin',(10.4681436286308,1.08420482079361,0.6));
#10518=CARTESIAN_POINT('Origin',(10.4681436286308,1.08420482079362,0.6));
#10519=CARTESIAN_POINT('Origin',(0.3318563713692,-1.09142177001972,0.6));
#10520=CARTESIAN_POINT('',(0.3318563713692,-1.09142177001972,0.9));
#10521=CARTESIAN_POINT('',(0.308522637995069,-1.39004019713626,0.616809874278785));
#10522=CARTESIAN_POINT('Origin',(0.3318563713692,-1.09142177001972,0.6));
#10523=CARTESIAN_POINT('',(0.0322675109428289,-1.09142177001972,0.615700786872884));
#10524=CARTESIAN_POINT('Origin',(0.3318563713692,-1.09142177001972,0.6));
#10525=CARTESIAN_POINT('Origin',(0.331856371369201,-1.09142177001972,0.6));
#10526=CARTESIAN_POINT('Origin',(0.3318563713692,-0.7,0.6));
#10527=CARTESIAN_POINT('',(0.0322675109428288,-0.7,0.615700786872883));
#10528=CARTESIAN_POINT('',(0.3318563713692,-0.7,0.9));
#10529=CARTESIAN_POINT('Ctrl Pts',(0.276048389810261,-1.42252533450788,
-0.00533608639730399));
#10530=CARTESIAN_POINT('Ctrl Pts',(0.28687338241706,-1.4116967417008,0.202045878554724));
#10531=CARTESIAN_POINT('Ctrl Pts',(0.297698133178874,-1.40086836142621,
0.409427865329919));
#10532=CARTESIAN_POINT('Ctrl Pts',(0.308522637995069,-1.39004019713626,
0.616809874278785));
#10533=CARTESIAN_POINT('Ctrl Pts',(0.191246496057484,-1.41570630783033,
-0.00124775669238285));
#10534=CARTESIAN_POINT('Ctrl Pts',(0.202080757839133,-1.40486573978029,
0.206133102090467));
#10535=CARTESIAN_POINT('Ctrl Pts',(0.212914648880055,-1.39402634701096,
0.413514041581016));
#10536=CARTESIAN_POINT('Ctrl Pts',(0.223748532748767,-1.38318608000504,
0.620894932085382));
#10537=CARTESIAN_POINT('Ctrl Pts',(0.0492682973509243,-1.33685850703924,
0.00207719607616587));
#10538=CARTESIAN_POINT('Ctrl Pts',(0.0601266125734448,-1.32601270457081,
0.209456583216085));
#10539=CARTESIAN_POINT('Ctrl Pts',(0.0709850253737815,-1.3151666447344,
0.416835949794532));
#10540=CARTESIAN_POINT('Ctrl Pts',(0.0818432319483421,-1.30432109509162,
0.624215353109623));
#10541=CARTESIAN_POINT('Ctrl Pts',(-0.000163444061205068,-1.18769013309795,
-0.00311869847265479));
#10542=CARTESIAN_POINT('Ctrl Pts',(0.0107049555364969,-1.17685886333949,
0.204261034729081));
#10543=CARTESIAN_POINT('Ctrl Pts',(0.0215730900970294,-1.16602762920277,
0.411640782964944));
#10544=CARTESIAN_POINT('Ctrl Pts',(0.0324414916763936,-1.15519677672624,
0.619020537031064));
#10545=CARTESIAN_POINT('Ctrl Pts',(-0.00033748371827097,-1.12389640457412,
-0.0064395729582146));
#10546=CARTESIAN_POINT('Ctrl Pts',(0.0105308471731094,-1.11307128361434,
0.200940534347673));
#10547=CARTESIAN_POINT('Ctrl Pts',(0.0213991787230862,-1.10224640406117,
0.408320654220332));
#10548=CARTESIAN_POINT('Ctrl Pts',(0.0322675109428289,-1.09142177001972,
0.615700786872884));
#10549=CARTESIAN_POINT('Ctrl Pts',(0.27632692456468,-1.42224670711126,5.13911829758129E-17));
#10550=CARTESIAN_POINT('Ctrl Pts',(0.287059068122268,-1.41151099373342,
0.20560326985903));
#10551=CARTESIAN_POINT('Ctrl Pts',(0.297790973931072,-1.40077548928706,
0.411206561171438));
#10552=CARTESIAN_POINT('Ctrl Pts',(0.308522637995069,-1.39004019713626,
0.616809874278785));
#10553=CARTESIAN_POINT('Ctrl Pts',(0.0322675109428289,-1.09142177001972,
0.615700786872884));
#10554=CARTESIAN_POINT('Ctrl Pts',(0.0215116733095221,-1.10213436178043,
0.410467178800746));
#10555=CARTESIAN_POINT('Ctrl Pts',(0.0107558363321879,-1.11284719399673,
0.205233583245308));
#10556=CARTESIAN_POINT('Ctrl Pts',(1.76901136968166E-16,-1.12356026268968,
-7.45931094670027E-17));
#10557=CARTESIAN_POINT('Origin',(10.4681436286308,-1.08420482109828,0.6));
#10558=CARTESIAN_POINT('',(10.7677324890572,-1.08420482079361,0.615700786872884));
#10559=CARTESIAN_POINT('',(10.4844020137689,-1.3833101379008,0.616482542003833));
#10560=CARTESIAN_POINT('Origin',(10.4681436286308,-1.08420482079361,0.600000000000001));
#10561=CARTESIAN_POINT('',(10.4681436258201,-1.08420482094639,0.9));
#10562=CARTESIAN_POINT('Origin',(10.4681436286308,-1.08420482109828,0.6));
#10563=CARTESIAN_POINT('Origin',(10.4681436286308,-1.08420482079361,0.6));
#10564=CARTESIAN_POINT('Origin',(10.4681436286308,0.7,0.6));
#10565=CARTESIAN_POINT('',(10.7677324890572,0.7,0.615700786872884));
#10566=CARTESIAN_POINT('',(10.4681436286308,0.7,0.9));
#10567=CARTESIAN_POINT('Ctrl Pts',(10.4681436286308,-1.08420482079361,0.9));
#10568=CARTESIAN_POINT('Ctrl Pts',(9.02115959826777,-1.16285813221549,0.9));
#10569=CARTESIAN_POINT('Ctrl Pts',(5.64262097844114,-1.30550334054488,0.9));
#10570=CARTESIAN_POINT('Ctrl Pts',(2.25816172369615,-1.24194126716656,0.9));
#10571=CARTESIAN_POINT('Ctrl Pts',(0.331856371369198,-1.09142177001972,
0.9));
#10572=CARTESIAN_POINT('Ctrl Pts',(10.4728449957889,-1.17069581622255,0.9));
#10573=CARTESIAN_POINT('Ctrl Pts',(9.02515960257209,-1.24945398332951,0.900002463983243));
#10574=CARTESIAN_POINT('Ctrl Pts',(5.64406008560805,-1.39235654229312,0.899995181674544));
#10575=CARTESIAN_POINT('Ctrl Pts',(2.25481214769604,-1.3286896492945,0.900006992415263));
#10576=CARTESIAN_POINT('Ctrl Pts',(0.325113511056834,-1.17771496230318,
0.9));
#10577=CARTESIAN_POINT('Ctrl Pts',(10.4809942371438,-1.32061731204901,0.830050158657121));
#10578=CARTESIAN_POINT('Ctrl Pts',(9.03210079995546,-1.3995487214628,0.829938185878055));
#10579=CARTESIAN_POINT('Ctrl Pts',(5.64656962219688,-1.54290142969263,0.82970437227026));
#10580=CARTESIAN_POINT('Ctrl Pts',(2.24896854757963,-1.47903552984056,0.829838703712927));
#10581=CARTESIAN_POINT('Ctrl Pts',(0.313425270489114,-1.32729771265557,
0.830156825336737));
#10582=CARTESIAN_POINT('Ctrl Pts',(10.4842082875648,-1.37974615923803,0.681348425135383));
#10583=CARTESIAN_POINT('Ctrl Pts',(9.03482793853036,-1.45862084618981,0.681058092399338));
#10584=CARTESIAN_POINT('Ctrl Pts',(5.64753778607331,-1.60187726023264,0.68045297450285));
#10585=CARTESIAN_POINT('Ctrl Pts',(2.24670449952385,-1.53809938127555,0.680799765935021));
#10586=CARTESIAN_POINT('Ctrl Pts',(0.308806004580392,-1.38641375285276,
0.681625057916928));
#10587=CARTESIAN_POINT('Ctrl Pts',(10.4844020137689,-1.3833101379008,0.616482542003833));
#10588=CARTESIAN_POINT('Ctrl Pts',(9.03499042108131,-1.46211428773623,0.616139856494792));
#10589=CARTESIAN_POINT('Ctrl Pts',(5.64759185703765,-1.60522711936681,0.615422163720642));
#10590=CARTESIAN_POINT('Ctrl Pts',(2.24657199659733,-1.54153220865049,0.615835494619844));
#10591=CARTESIAN_POINT('Ctrl Pts',(0.308522637995066,-1.39004019713626,
0.616809874278785));
#10592=CARTESIAN_POINT('Ctrl Pts',(0.308522637995066,-1.39004019713626,
0.616809874278785));
#10593=CARTESIAN_POINT('Ctrl Pts',(2.24657199659733,-1.54153220865049,0.615835494619844));
#10594=CARTESIAN_POINT('Ctrl Pts',(5.64759185703765,-1.60522711936681,0.615422163720642));
#10595=CARTESIAN_POINT('Ctrl Pts',(9.03499042108131,-1.46211428773623,0.616139856494792));
#10596=CARTESIAN_POINT('Ctrl Pts',(10.4844020137689,-1.3833101379008,0.616482542003833));
#10597=CARTESIAN_POINT('Ctrl Pts',(10.4681436258201,-1.08420482094639,0.900000000000001));
#10598=CARTESIAN_POINT('Ctrl Pts',(9.02115959639274,-1.16285813229465,0.9));
#10599=CARTESIAN_POINT('Ctrl Pts',(5.64262097750198,-1.30550334052724,0.9));
#10600=CARTESIAN_POINT('Ctrl Pts',(2.25816172369615,-1.24194126716656,0.9));
#10601=CARTESIAN_POINT('Ctrl Pts',(0.331856371369198,-1.09142177001972,
0.9));
#10602=CARTESIAN_POINT('Ctrl Pts',(10.8003433549902,-1.11672267507076,-0.00655160349952438));
#10603=CARTESIAN_POINT('Ctrl Pts',(10.7894730668347,-1.10588321133639,0.200865850630566));
#10604=CARTESIAN_POINT('Ctrl Pts',(10.7786027781932,-1.09504392553578,0.408283314033857));
#10605=CARTESIAN_POINT('Ctrl Pts',(10.7677324890572,-1.08420482079361,0.615700786872885));
#10606=CARTESIAN_POINT('Ctrl Pts',(10.8001073672393,-1.20312439623403,-0.00204868896805508));
#10607=CARTESIAN_POINT('Ctrl Pts',(10.7892368724076,-1.19227880391739,0.205368384315645));
#10608=CARTESIAN_POINT('Ctrl Pts',(10.7783670568079,-1.18143370221047,0.41278551899075));
#10609=CARTESIAN_POINT('Ctrl Pts',(10.7674965587017,-1.17058839661753,0.620202606234566));
#10610=CARTESIAN_POINT('Ctrl Pts',(10.7300137544668,-1.35289768637741,0.00210488808650419));
#10611=CARTESIAN_POINT('Ctrl Pts',(10.7191538066016,-1.34204221082848,0.209521911971666));
#10612=CARTESIAN_POINT('Ctrl Pts',(10.7082938463195,-1.33118673671862,0.416938933985702));
#10613=CARTESIAN_POINT('Ctrl Pts',(10.6974340169938,-1.32033143065575,0.624355970618915));
#10614=CARTESIAN_POINT('Ctrl Pts',(10.5816241002662,-1.4121605627967,-0.00257485550010117));
#10615=CARTESIAN_POINT('Ctrl Pts',(10.5707805459565,-1.4013126969686,0.204843391064434));
#10616=CARTESIAN_POINT('Ctrl Pts',(10.5599369567012,-1.39046512672587,0.412261650129749));
#10617=CARTESIAN_POINT('Ctrl Pts',(10.5490937145378,-1.37961751361469,0.619679923312015));
#10618=CARTESIAN_POINT('Ctrl Pts',(10.5169176890673,-1.41583338198674,-0.00577403633861717));
#10619=CARTESIAN_POINT('Ctrl Pts',(10.5060789456421,-1.40499213715574,0.201644806368331));
#10620=CARTESIAN_POINT('Ctrl Pts',(10.4952403861233,-1.39415105487295,0.40906366572247));
#10621=CARTESIAN_POINT('Ctrl Pts',(10.4844020137689,-1.3833101379008,0.616482542003833));
#10622=CARTESIAN_POINT('Ctrl Pts',(10.8,-1.11638029377732,-2.51534904016637E-17));
#10623=CARTESIAN_POINT('Ctrl Pts',(10.7892441634977,-1.10565496086826,0.205233586491178));
#10624=CARTESIAN_POINT('Ctrl Pts',(10.7784883265195,-1.09492980219801,0.410467182062988));
#10625=CARTESIAN_POINT('Ctrl Pts',(10.7677324890572,-1.08420482079361,0.615700786872885));
#10626=CARTESIAN_POINT('Ctrl Pts',(10.4844020137689,-1.3833101379008,0.616482542003833));
#10627=CARTESIAN_POINT('Ctrl Pts',(10.4951398148107,-1.39405045994841,0.410988344812119));
#10628=CARTESIAN_POINT('Ctrl Pts',(10.5058777995597,-1.40479094425298,0.205494164234945));
#10629=CARTESIAN_POINT('Ctrl Pts',(10.5166159648474,-1.4155315881283,-2.5652223401007E-16));
#10630=CARTESIAN_POINT('Ctrl Pts',(10.5169125872774,1.41582827901939,-0.0056764044152427));
#10631=CARTESIAN_POINT('Ctrl Pts',(10.5060755445066,1.40498873522851,0.20170989432247));
#10632=CARTESIAN_POINT('Ctrl Pts',(10.4952386855848,1.39414935393528,0.409096209702196));
#10633=CARTESIAN_POINT('Ctrl Pts',(10.4844020137689,1.3833101379008,0.616482542003833));
#10634=CARTESIAN_POINT('Ctrl Pts',(10.6031877991504,1.41093118264609,-0.00141083033817288));
#10635=CARTESIAN_POINT('Ctrl Pts',(10.5923442181457,1.40008262840665,0.205974657203891));
#10636=CARTESIAN_POINT('Ctrl Pts',(10.5815009048179,1.38923496752292,0.413360205434192));
#10637=CARTESIAN_POINT('Ctrl Pts',(10.5706576147941,1.37838663885266,0.62074571708141));
#10638=CARTESIAN_POINT('Ctrl Pts',(10.7489822201969,1.33286898269122,0.00215046584238339));
#10639=CARTESIAN_POINT('Ctrl Pts',(10.7381210493968,1.32201618867047,0.209534855263179));
#10640=CARTESIAN_POINT('Ctrl Pts',(10.7272598662103,1.31116338896628,0.416919242515175));
#10641=CARTESIAN_POINT('Ctrl Pts',(10.716398780155,1.30031077634578,0.624303643734563));
#10642=CARTESIAN_POINT('Ctrl Pts',(10.8001612475457,1.18151886169146,-0.00307678645922502));
#10643=CARTESIAN_POINT('Ctrl Pts',(10.7892926103682,1.17067663552019,0.20430785074418));
#10644=CARTESIAN_POINT('Ctrl Pts',(10.7784241800195,1.15983442267521,0.41169249890798));
#10645=CARTESIAN_POINT('Ctrl Pts',(10.7675555412906,1.14899250266155,0.619077151394146));
#10646=CARTESIAN_POINT('Ctrl Pts',(10.8003382383521,1.11671757294177,-0.00645397222975308));
#10647=CARTESIAN_POINT('Ctrl Pts',(10.7894696557425,1.1058798099729,0.200930938146656));
#10648=CARTESIAN_POINT('Ctrl Pts',(10.778601072647,1.09504222488243,0.408315857793383));
#10649=CARTESIAN_POINT('Ctrl Pts',(10.7677324890572,1.08420482079361,0.615700786872884));
#10650=CARTESIAN_POINT('Ctrl Pts',(10.5166159648474,1.4155315881283,3.37837396946483E-16));
#10651=CARTESIAN_POINT('Ctrl Pts',(10.5058777995597,1.40479094425298,0.205494164234944));
#10652=CARTESIAN_POINT('Ctrl Pts',(10.4951398148107,1.39405045994841,0.41098834481212));
#10653=CARTESIAN_POINT('Ctrl Pts',(10.4844020137689,1.3833101379008,0.616482542003833));
#10654=CARTESIAN_POINT('Ctrl Pts',(10.7677324890572,1.08420482079361,0.615700786872884));
#10655=CARTESIAN_POINT('Ctrl Pts',(10.7784883265195,1.09492980219801,0.410467182062988));
#10656=CARTESIAN_POINT('Ctrl Pts',(10.7892441634977,1.10565496086826,0.205233586491177));
#10657=CARTESIAN_POINT('Ctrl Pts',(10.8,1.11638029377732,-4.7271214720368E-17));
#10658=CARTESIAN_POINT('Ctrl Pts',(0.3318563713692,1.09142177001972,0.9));
#10659=CARTESIAN_POINT('Ctrl Pts',(1.77658538561441,1.20431139287985,0.9));
#10660=CARTESIAN_POINT('Ctrl Pts',(5.15852145577913,1.31798734362749,0.900000000000001));
#10661=CARTESIAN_POINT('Ctrl Pts',(8.53883158814675,1.18907590268945,0.9));
#10662=CARTESIAN_POINT('Ctrl Pts',(10.4681436286308,1.08420482079361,0.9));
#10663=CARTESIAN_POINT('Ctrl Pts',(0.325113511056836,1.17771496230318,0.9));
#10664=CARTESIAN_POINT('Ctrl Pts',(1.77238748853623,1.29094597754667,0.900005244311447));
#10665=CARTESIAN_POINT('Ctrl Pts',(5.15940689953628,1.40489117512763,0.899995532233175));
#10666=CARTESIAN_POINT('Ctrl Pts',(8.54259780483314,1.2757067056985,0.90000328531099));
#10667=CARTESIAN_POINT('Ctrl Pts',(10.4728449957889,1.17069581622255,0.9));
#10668=CARTESIAN_POINT('Ctrl Pts',(0.313425270489116,1.32729771265557,0.830156825336737));
#10669=CARTESIAN_POINT('Ctrl Pts',(1.76508272830699,1.44110107554431,0.829918234118879));
#10670=CARTESIAN_POINT('Ctrl Pts',(5.16095094050242,1.55552201031752,0.829677185710002));
#10671=CARTESIAN_POINT('Ctrl Pts',(8.54913632089268,1.4258591912674,0.829900861618366));
#10672=CARTESIAN_POINT('Ctrl Pts',(10.4809942371438,1.32061731204901,0.830050158657121));
#10673=CARTESIAN_POINT('Ctrl Pts',(0.308806004580394,1.38641375285276,0.681625057916928));
#10674=CARTESIAN_POINT('Ctrl Pts',(1.76222987578798,1.50017797416985,0.681006088930498));
#10675=CARTESIAN_POINT('Ctrl Pts',(5.16154986224672,1.61450132085358,0.68038246417749));
#10676=CARTESIAN_POINT('Ctrl Pts',(8.55170115551887,1.48491240850707,0.680961314820656));
#10677=CARTESIAN_POINT('Ctrl Pts',(10.4842082875648,1.37974615923803,0.681348425135383));
#10678=CARTESIAN_POINT('Ctrl Pts',(0.308522637995068,1.39004019713626,0.616809874278785));
#10679=CARTESIAN_POINT('Ctrl Pts',(1.76205965694675,1.50365920577193,0.616079089534579));
#10680=CARTESIAN_POINT('Ctrl Pts',(5.16158497046229,1.61783515152865,0.615338844765104));
#10681=CARTESIAN_POINT('Ctrl Pts',(8.55185322351876,1.48838233768137,0.616025627991778));
#10682=CARTESIAN_POINT('Ctrl Pts',(10.4844020137689,1.3833101379008,0.616482542003833));
#10683=CARTESIAN_POINT('Ctrl Pts',(10.4844020137689,1.3833101379008,0.616482542003833));
#10684=CARTESIAN_POINT('Ctrl Pts',(8.55185322351876,1.48838233768137,0.616025627991778));
#10685=CARTESIAN_POINT('Ctrl Pts',(5.16158497046229,1.61783515152865,0.615338844765104));
#10686=CARTESIAN_POINT('Ctrl Pts',(1.76205965694675,1.50365920577193,0.616079089534579));
#10687=CARTESIAN_POINT('Ctrl Pts',(0.308522637995068,1.39004019713626,0.616809874278785));
#10688=CARTESIAN_POINT('Ctrl Pts',(0.3318563713692,1.09142177001972,0.9));
#10689=CARTESIAN_POINT('Ctrl Pts',(1.77658538561441,1.20431139287985,0.9));
#10690=CARTESIAN_POINT('Ctrl Pts',(5.15852145577913,1.31798734362749,0.900000000000001));
#10691=CARTESIAN_POINT('Ctrl Pts',(8.53883158814675,1.18907590268945,0.9));
#10692=CARTESIAN_POINT('Ctrl Pts',(10.4681436286308,1.08420482079361,0.9));
#10693=CARTESIAN_POINT('Ctrl Pts',(-0.000344602063817145,1.12390349461883,
-0.00657539908256866));
#10694=CARTESIAN_POINT('Ctrl Pts',(0.0105261016091243,1.11307601020539,
0.200849983592616));
#10695=CARTESIAN_POINT('Ctrl Pts',(0.0213968059409475,1.10224876730309,
0.408275378840013));
#10696=CARTESIAN_POINT('Ctrl Pts',(0.0322675109428289,1.09142177001972,
0.615700786872884));
#10697=CARTESIAN_POINT('Ctrl Pts',(-0.000112549170678945,1.2089618047365,
-0.00214756610981592));
#10698=CARTESIAN_POINT('Ctrl Pts',(0.0107584275574203,1.19812589474889,
0.205277296000037));
#10699=CARTESIAN_POINT('Ctrl Pts',(0.021628504370896,1.18729063034778,0.412702239156743));
#10700=CARTESIAN_POINT('Ctrl Pts',(0.0324994852542487,1.17645511229507,
0.620127120417125));
#10701=CARTESIAN_POINT('Ctrl Pts',(0.0675181008536004,1.35659180908255,
0.00201426213057289));
#10702=CARTESIAN_POINT('Ctrl Pts',(0.0783748317004002,1.34574224493831,
0.20943904356877));
#10703=CARTESIAN_POINT('Ctrl Pts',(0.0892318011706237,1.33489254525337,
0.416863803530356));
#10704=CARTESIAN_POINT('Ctrl Pts',(0.100088380073201,1.32404321751407,0.624288602298589));
#10705=CARTESIAN_POINT('Ctrl Pts',(0.212439875011655,1.41741816253371,-0.00240566592686199));
#10706=CARTESIAN_POINT('Ctrl Pts',(0.223274062163905,1.40657840226088,0.20502076110302));
#10707=CARTESIAN_POINT('Ctrl Pts',(0.234108278795672,1.39573903465802,0.412447205628077));
#10708=CARTESIAN_POINT('Ctrl Pts',(0.244942059060342,1.38489960928785,0.619873667633733));
#10709=CARTESIAN_POINT('Ctrl Pts',(0.276041299849618,1.42253242682652,-0.00547191373834488));
#10710=CARTESIAN_POINT('Ctrl Pts',(0.286868655882245,1.41170146982041,0.201955326984501));
#10711=CARTESIAN_POINT('Ctrl Pts',(0.297695769965166,1.40087072543886,0.409382589539965));
#10712=CARTESIAN_POINT('Ctrl Pts',(0.308522637995069,1.39004019713626,0.616809874278785));
#10713=CARTESIAN_POINT('Ctrl Pts',(2.26869304592592E-17,1.12356026268968,
-3.16587034365767E-17));
#10714=CARTESIAN_POINT('Ctrl Pts',(0.0107558363321878,1.11284719399672,
0.205233583245308));
#10715=CARTESIAN_POINT('Ctrl Pts',(0.0215116733095221,1.10213436178043,
0.410467178800746));
#10716=CARTESIAN_POINT('Ctrl Pts',(0.0322675109428289,1.09142177001972,
0.615700786872884));
#10717=CARTESIAN_POINT('Ctrl Pts',(0.308522637995069,1.39004019713626,0.616809874278785));
#10718=CARTESIAN_POINT('Ctrl Pts',(0.297790973931072,1.40077548928706,0.411206561171438));
#10719=CARTESIAN_POINT('Ctrl Pts',(0.287059068122271,1.41151099373341,0.205603269859031));
#10720=CARTESIAN_POINT('Ctrl Pts',(0.276326924564681,1.42224670711126,-2.68882138776405E-16));
#10721=CARTESIAN_POINT('Ctrl Pts',(10.5166159648474,-1.4155315881283,0.));
#10722=CARTESIAN_POINT('Ctrl Pts',(10.5064062201588,-1.40475637621136,0.205603291426271));
#10723=CARTESIAN_POINT('Ctrl Pts',(10.4961964754701,-1.39398116429443,0.411206582852543));
#10724=CARTESIAN_POINT('Ctrl Pts',(10.4859867307814,-1.38320595237749,0.616809874278814));
#10725=CARTESIAN_POINT('Ctrl Pts',(7.10318628475318,-1.599994843061,0.));
#10726=CARTESIAN_POINT('Ctrl Pts',(7.09978773046573,-1.58921963114407,0.205603291426271));
#10727=CARTESIAN_POINT('Ctrl Pts',(7.09638917617828,-1.57844441922713,0.411206582852543));
#10728=CARTESIAN_POINT('Ctrl Pts',(7.09299062189083,-1.5676692073102,0.616809874278814));
#10729=CARTESIAN_POINT('Ctrl Pts',(3.68975660465893,-1.68747752195839,0.));
#10730=CARTESIAN_POINT('Ctrl Pts',(3.69316924077269,-1.67670231004145,0.205603291426272));
#10731=CARTESIAN_POINT('Ctrl Pts',(3.69658187688646,-1.66592709812452,0.411206582852543));
#10732=CARTESIAN_POINT('Ctrl Pts',(3.69999451300023,-1.65515188620758,0.616809874278814));
#10733=CARTESIAN_POINT('Ctrl Pts',(0.276326924564679,-1.42224670711126,
0.));
#10734=CARTESIAN_POINT('Ctrl Pts',(0.286550751079662,-1.41147149519433,
0.205603291426271));
#10735=CARTESIAN_POINT('Ctrl Pts',(0.296774577594646,-1.40069628327739,
0.411206582852543));
#10736=CARTESIAN_POINT('Ctrl Pts',(0.306998404109629,-1.38992107136046,
0.616809874278814));
#10737=CARTESIAN_POINT('Origin',(0.,-1.4,0.));
#10738=CARTESIAN_POINT('Origin',(5.4,-8.13935059369636E-18,0.9));
#10739=CARTESIAN_POINT('Ctrl Pts',(0.276326924564679,1.42224670711126,0.));
#10740=CARTESIAN_POINT('Ctrl Pts',(0.286550751079662,1.41147149519433,0.205603291426271));
#10741=CARTESIAN_POINT('Ctrl Pts',(0.296774577594645,1.40069628327739,0.411206582852543));
#10742=CARTESIAN_POINT('Ctrl Pts',(0.306998404109628,1.38992107136046,0.616809874278814));
#10743=CARTESIAN_POINT('Ctrl Pts',(3.68975660465893,1.68747752195839,0.));
#10744=CARTESIAN_POINT('Ctrl Pts',(3.6931692407727,1.67670231004145,0.205603291426271));
#10745=CARTESIAN_POINT('Ctrl Pts',(3.69658187688646,1.66592709812452,0.411206582852543));
#10746=CARTESIAN_POINT('Ctrl Pts',(3.69999451300023,1.65515188620758,0.616809874278814));
#10747=CARTESIAN_POINT('Ctrl Pts',(7.10318628475318,1.599994843061,0.));
#10748=CARTESIAN_POINT('Ctrl Pts',(7.09978773046573,1.58921963114407,0.205603291426271));
#10749=CARTESIAN_POINT('Ctrl Pts',(7.09638917617828,1.57844441922713,0.411206582852543));
#10750=CARTESIAN_POINT('Ctrl Pts',(7.09299062189083,1.5676692073102,0.616809874278814));
#10751=CARTESIAN_POINT('Ctrl Pts',(10.5166159648474,1.4155315881283,0.));
#10752=CARTESIAN_POINT('Ctrl Pts',(10.5064062201588,1.40475637621136,0.205603291426271));
#10753=CARTESIAN_POINT('Ctrl Pts',(10.4961964754701,1.39398116429443,0.411206582852543));
#10754=CARTESIAN_POINT('Ctrl Pts',(10.4859867307814,1.38320595237749,0.616809874278814));
#10755=CARTESIAN_POINT('Origin',(10.8,1.4,0.));
#10756=CARTESIAN_POINT('',(0.,0.,0.));
#10757=CARTESIAN_POINT('Origin',(8.1,-1.,0.7));
#10758=CARTESIAN_POINT('',(7.94916965151797,-1.19937453693185,0.7));
#10759=CARTESIAN_POINT('',(8.26514540988519,-1.18768855477586,0.7));
#10760=CARTESIAN_POINT('Ctrl Pts',(7.94916965151797,-1.19937453693185,0.7));
#10761=CARTESIAN_POINT('Ctrl Pts',(7.97160858810976,-1.21634998764782,0.7));
#10762=CARTESIAN_POINT('Ctrl Pts',(7.99739856866269,-1.22989011121344,0.69528529300377));
#10763=CARTESIAN_POINT('Ctrl Pts',(8.03944443766207,-1.24298414277179,0.688517705185315));
#10764=CARTESIAN_POINT('Ctrl Pts',(8.05362924383607,-1.24609346022897,0.686388676887586));
#10765=CARTESIAN_POINT('Ctrl Pts',(8.075506183533,-1.24890990228851,0.684139035126277));
#10766=CARTESIAN_POINT('Ctrl Pts',(8.08297567221474,-1.24953307703463,0.683546226354886));
#10767=CARTESIAN_POINT('Ctrl Pts',(8.0940066533036,-1.24995288972095,0.68299521602547));
#10768=CARTESIAN_POINT('Ctrl Pts',(8.09752287926269,-1.25001251279495,0.68286729538075));
#10769=CARTESIAN_POINT('Ctrl Pts',(8.10293413375911,-1.249989933108,0.682747340264197));
#10770=CARTESIAN_POINT('Ctrl Pts',(8.10482478940148,-1.24996059450444,0.682719828470948));
#10771=CARTESIAN_POINT('Ctrl Pts',(8.10828546792054,-1.24986760009171,0.682696100760705));
#10772=CARTESIAN_POINT('Ctrl Pts',(8.10985478687837,-1.24981062779486,0.682695370268813));
#10773=CARTESIAN_POINT('Ctrl Pts',(8.11326464342549,-1.24965465239671,0.682715595753076));
#10774=CARTESIAN_POINT('Ctrl Pts',(8.11510409202247,-1.2495501177419,0.682740330911594));
#10775=CARTESIAN_POINT('Ctrl Pts',(8.12014207260669,-1.24920790966494,0.682845651127781));
#10776=CARTESIAN_POINT('Ctrl Pts',(8.12333423895876,-1.24892926854386,0.682953992816581));
#10777=CARTESIAN_POINT('Ctrl Pts',(8.139194120874,-1.2472372768871,0.683691668462565));
#10778=CARTESIAN_POINT('Ctrl Pts',(8.15164141295685,-1.2449338270761,0.684918799511701));
#10779=CARTESIAN_POINT('Ctrl Pts',(8.19196937649467,-1.23428099896052,0.690212518998986));
#10780=CARTESIAN_POINT('Ctrl Pts',(8.21811504697062,-1.22213176592155,0.695755006185672));
#10781=CARTESIAN_POINT('Ctrl Pts',(8.24962874265135,-1.20052913769617,0.699397421419897));
#10782=CARTESIAN_POINT('Ctrl Pts',(8.25758631484639,-1.19433973204149,0.7));
#10783=CARTESIAN_POINT('Ctrl Pts',(8.26514540988519,-1.18768855477586,0.7));
#10784=CARTESIAN_POINT('Origin',(8.1,-1.,0.7));
#10785=CARTESIAN_POINT('Origin',(2.7,1.,0.7));
#10786=CARTESIAN_POINT('',(2.8076286513348,1.22564590451442,0.7));
#10787=CARTESIAN_POINT('',(2.57739843082973,1.21787348447435,0.7));
#10788=CARTESIAN_POINT('Ctrl Pts',(2.80762864495888,1.22564590575571,0.7));
#10789=CARTESIAN_POINT('Ctrl Pts',(2.78743249310418,1.23527907171202,0.7));
#10790=CARTESIAN_POINT('Ctrl Pts',(2.76507271635938,1.24261561512899,0.698430289974852));
#10791=CARTESIAN_POINT('Ctrl Pts',(2.73219941643314,1.24807722603274,0.696876198609429));
#10792=CARTESIAN_POINT('Ctrl Pts',(2.72335305886828,1.24906618730719,0.696525251810408));
#10793=CARTESIAN_POINT('Ctrl Pts',(2.71018695034311,1.24982905432238,0.696188910804419));
#10794=CARTESIAN_POINT('Ctrl Pts',(2.70590779780308,1.24996687586326,0.696107915309552));
#10795=CARTESIAN_POINT('Ctrl Pts',(2.69921702211412,1.25001037316246,0.696030339680738));
#10796=CARTESIAN_POINT('Ctrl Pts',(2.69680890442544,1.24999123464332,0.696012302673685));
#10797=CARTESIAN_POINT('Ctrl Pts',(2.69234597975348,1.24989125947742,0.695997601992606));
#10798=CARTESIAN_POINT('Ctrl Pts',(2.69029169500035,1.24981988388707,0.69599819279703));
#10799=CARTESIAN_POINT('Ctrl Pts',(2.6857660481318,1.24960673159635,0.696015705561832));
#10800=CARTESIAN_POINT('Ctrl Pts',(2.68329599580702,1.24945360531346,0.696035938105249));
#10801=CARTESIAN_POINT('Ctrl Pts',(2.67625328071593,1.24891193026541,0.696123377063474));
#10802=CARTESIAN_POINT('Ctrl Pts',(2.67169109188753,1.24843439216159,0.696216059649547));
#10803=CARTESIAN_POINT('Ctrl Pts',(2.64765560351845,1.24524789167778,0.696873729305584));
#10804=CARTESIAN_POINT('Ctrl Pts',(2.62857598726268,1.24037162800668,0.698048768812303));
#10805=CARTESIAN_POINT('Ctrl Pts',(2.59902076831046,1.22902239593109,0.699541037747764));
#10806=CARTESIAN_POINT('Ctrl Pts',(2.58799157881597,1.22383445108162,0.7));
#10807=CARTESIAN_POINT('Ctrl Pts',(2.57739843082979,1.21787348447436,0.7));
#10808=CARTESIAN_POINT('Origin',(2.7,1.,0.7));
#10809=CARTESIAN_POINT('Origin',(2.7,-1.,0.7));
#10810=CARTESIAN_POINT('',(2.57739843082979,-1.21787348447436,0.7));
#10811=CARTESIAN_POINT('',(2.80762864495888,-1.22564590575571,0.7));
#10812=CARTESIAN_POINT('Ctrl Pts',(2.57739843082979,-1.21787348447436,0.7));
#10813=CARTESIAN_POINT('Ctrl Pts',(2.59689796709118,-1.22884624579732,0.7));
#10814=CARTESIAN_POINT('Ctrl Pts',(2.61871070177046,-1.23767364961455,0.698430520021629));
#10815=CARTESIAN_POINT('Ctrl Pts',(2.6511387549791,-1.24533993869645,0.696876447160353));
#10816=CARTESIAN_POINT('Ctrl Pts',(2.65989793055836,-1.24692336726652,0.696525471319567));
#10817=CARTESIAN_POINT('Ctrl Pts',(2.67298219502323,-1.24857266139659,0.696189053183015));
#10818=CARTESIAN_POINT('Ctrl Pts',(2.67724223626036,-1.24899884484677,0.696108027479433));
#10819=CARTESIAN_POINT('Ctrl Pts',(2.68391475503581,-1.24949361628703,0.696030400846995));
#10820=CARTESIAN_POINT('Ctrl Pts',(2.68631866330158,-1.24963697932539,0.69601234479389));
#10821=CARTESIAN_POINT('Ctrl Pts',(2.69077815115796,-1.24983831390468,0.695997608323079));
#10822=CARTESIAN_POINT('Ctrl Pts',(2.69283257145917,-1.24990568929416,0.695998182544699));
#10823=CARTESIAN_POINT('Ctrl Pts',(2.69736230434386,-1.24999833696454,0.696015659042177));
#10824=CARTESIAN_POINT('Ctrl Pts',(2.69983707579759,-1.25001219669429,0.696035872086962));
#10825=CARTESIAN_POINT('Ctrl Pts',(2.70690037992806,-1.24994687665095,0.696123257636812));
#10826=CARTESIAN_POINT('Ctrl Pts',(2.71148446565418,-1.24977820005943,0.696215908504701));
#10827=CARTESIAN_POINT('Ctrl Pts',(2.73568105999059,-1.24822038288304,0.696873447340259));
#10828=CARTESIAN_POINT('Ctrl Pts',(2.75504695022812,-1.24464213141243,0.698048515307351));
#10829=CARTESIAN_POINT('Ctrl Pts',(2.78530198112344,-1.2353118289445,0.699540950501024));
#10830=CARTESIAN_POINT('Ctrl Pts',(2.79665680001786,-1.23087925931356,0.7));
#10831=CARTESIAN_POINT('Ctrl Pts',(2.80762864495888,-1.22564590575571,0.7));
#10832=CARTESIAN_POINT('Origin',(2.7,-1.,0.7));
#10833=CARTESIAN_POINT('Origin',(8.1,1.,0.7));
#10834=CARTESIAN_POINT('',(8.26514540988519,1.18768855477586,0.7));
#10835=CARTESIAN_POINT('',(7.94916965249954,1.19937453719419,0.7));
#10836=CARTESIAN_POINT('Ctrl Pts',(8.26514540988519,1.18768855477586,0.7));
#10837=CARTESIAN_POINT('Ctrl Pts',(8.24402114884725,1.20627559516199,0.7));
#10838=CARTESIAN_POINT('Ctrl Pts',(8.21930102059268,1.22168408824046,0.695284768760077));
#10839=CARTESIAN_POINT('Ctrl Pts',(8.17833936508797,1.23784683595578,0.688517484674842));
#10840=CARTESIAN_POINT('Ctrl Pts',(8.16442627443898,1.24199461640617,0.686388979601913));
#10841=CARTESIAN_POINT('Ctrl Pts',(8.14282164862934,1.24641910835203,0.684139556285851));
#10842=CARTESIAN_POINT('Ctrl Pts',(8.13541969045672,1.24759243465272,0.683546718614312));
#10843=CARTESIAN_POINT('Ctrl Pts',(8.12445132655127,1.24882623938238,0.682995554842566));
#10844=CARTESIAN_POINT('Ctrl Pts',(8.12094947916695,1.24914555886372,0.68286756899844));
#10845=CARTESIAN_POINT('Ctrl Pts',(8.11555178799172,1.24952297970176,0.682747494033431));
#10846=CARTESIAN_POINT('Ctrl Pts',(8.11366421100955,1.24963346420394,0.682719937279798));
#10847=CARTESIAN_POINT('Ctrl Pts',(8.11020620287515,1.24979651712922,0.682696124556263));
#10848=CARTESIAN_POINT('Ctrl Pts',(8.10863696767328,1.24985569708818,0.682695355189016));
#10849=CARTESIAN_POINT('Ctrl Pts',(8.10522484403353,1.249952190393,0.682715496638402));
#10850=CARTESIAN_POINT('Ctrl Pts',(8.10338263267786,1.24998390529834,0.682740187713169));
#10851=CARTESIAN_POINT('Ctrl Pts',(8.09833277498968,1.25001501472208,0.682845394223802));
#10852=CARTESIAN_POINT('Ctrl Pts',(8.09512844909059,1.24997307323179,0.682953673497893));
#10853=CARTESIAN_POINT('Ctrl Pts',(8.07918314804204,1.24945780552822,0.683691186949858));
#10854=CARTESIAN_POINT('Ctrl Pts',(8.06659630270856,1.24808001426183,0.684918585227095));
#10855=CARTESIAN_POINT('Ctrl Pts',(8.02558960427868,1.24043495378573,0.69021260546313));
#10856=CARTESIAN_POINT('Ctrl Pts',(7.9986188553413,1.2302509517108,0.695754623970086));
#10857=CARTESIAN_POINT('Ctrl Pts',(7.96559475436581,1.21103543221342,0.69939729083119));
#10858=CARTESIAN_POINT('Ctrl Pts',(7.95720051358587,1.20545002552208,0.7));
#10859=CARTESIAN_POINT('Ctrl Pts',(7.94916965151797,1.19937453693185,0.7));
#10860=CARTESIAN_POINT('Origin',(8.1,1.,0.7));
#10861=CARTESIAN_POINT('Ctrl Pts',(1.1,1.14549341399196,0.7));
#10862=CARTESIAN_POINT('Ctrl Pts',(1.89984199608574,1.1957170361627,0.7));
#10863=CARTESIAN_POINT('Ctrl Pts',(2.70080437300401,1.2273695200909,0.7));
#10864=CARTESIAN_POINT('Ctrl Pts',(3.50204003610941,1.24374118183538,0.7));
#10865=CARTESIAN_POINT('Ctrl Pts',(1.09819048660397,1.17431102498992,0.7));
#10866=CARTESIAN_POINT('Ctrl Pts',(1.89847848223077,1.22458382597074,0.70000077422621));
#10867=CARTESIAN_POINT('Ctrl Pts',(2.69984520196781,1.25626413437997,0.699999727319846));
#10868=CARTESIAN_POINT('Ctrl Pts',(3.50144932661635,1.27265074030048,0.700000000000001));
#10869=CARTESIAN_POINT('Ctrl Pts',(1.09505363188407,1.22426736091617,0.676703190608825));
#10870=CARTESIAN_POINT('Ctrl Pts',(1.89610976425884,1.27462253270773,0.67666760713801));
#10871=CARTESIAN_POINT('Ctrl Pts',(2.69818680938115,1.3063522351595,0.67664530655333));
#10872=CARTESIAN_POINT('Ctrl Pts',(3.50042536655637,1.322763754511,0.676632802377821));
#10873=CARTESIAN_POINT('Ctrl Pts',(1.09381704710221,1.24396073223232,0.627109609335854));
#10874=CARTESIAN_POINT('Ctrl Pts',(1.89518106151152,1.29430885982199,0.62701751976321));
#10875=CARTESIAN_POINT('Ctrl Pts',(2.69753328610131,1.32603127467068,0.626959208652505));
#10876=CARTESIAN_POINT('Ctrl Pts',(3.50002334924346,1.34243864233338,0.626926882269943));
#10877=CARTESIAN_POINT('Ctrl Pts',(1.09374258853658,1.24514653057163,0.605486452199395));
#10878=CARTESIAN_POINT('Ctrl Pts',(1.89512529323683,1.29547288309274,0.605377720397184));
#10879=CARTESIAN_POINT('Ctrl Pts',(2.69749615303001,1.32718177535833,0.605308474776761));
#10880=CARTESIAN_POINT('Ctrl Pts',(3.5,1.34358136363184,0.605270327458635));
#10881=CARTESIAN_POINT('',(1.1,1.14549341399195,0.7));
#10882=CARTESIAN_POINT('Ctrl Pts',(1.1,1.14549341399196,0.7));
#10883=CARTESIAN_POINT('Ctrl Pts',(1.59210562457523,1.17639367564078,0.7));
#10884=CARTESIAN_POINT('Ctrl Pts',(2.08463535466703,1.20026407570248,0.7));
#10885=CARTESIAN_POINT('Ctrl Pts',(2.57739190516306,1.2178709162388,0.7));
#10886=CARTESIAN_POINT('',(1.1,1.24553911298206,0.605485603995113));
#10887=CARTESIAN_POINT('Ctrl Pts',(1.1,1.14549341399196,0.7));
#10888=CARTESIAN_POINT('Ctrl Pts',(1.1,1.15341616150799,0.7));
#10889=CARTESIAN_POINT('Ctrl Pts',(1.1000012416168,1.16127613060545,0.699006361583129));
#10890=CARTESIAN_POINT('Ctrl Pts',(1.10000231308998,1.16893252943985,0.697119293189023));
#10891=CARTESIAN_POINT('Ctrl Pts',(1.10000291357081,1.17322337016277,0.696061732044743));
#10892=CARTESIAN_POINT('Ctrl Pts',(1.10000345673767,1.17745032641463,0.694722535963768));
#10893=CARTESIAN_POINT('Ctrl Pts',(1.10000379529503,1.18158693416151,0.693112479763539));
#10894=CARTESIAN_POINT('Ctrl Pts',(1.1000044034764,1.18901789868739,0.690220189452084));
#10895=CARTESIAN_POINT('Ctrl Pts',(1.1000042334852,1.19607766167095,0.686488065947256));
#10896=CARTESIAN_POINT('Ctrl Pts',(1.10000339376692,1.2026196529327,0.681996646156542));
#10897=CARTESIAN_POINT('Ctrl Pts',(1.10000293249552,1.20621327895058,0.67952943359521));
#10898=CARTESIAN_POINT('Ctrl Pts',(1.10000228571683,1.20965039763183,0.676832226278619));
#10899=CARTESIAN_POINT('Ctrl Pts',(1.10000171524363,1.21290279159005,0.673912896410569));
#10900=CARTESIAN_POINT('Ctrl Pts',(1.10000115816795,1.2160788033717,0.671062126739188));
#10901=CARTESIAN_POINT('Ctrl Pts',(1.10000066850715,1.2190594221245,0.668016750164662));
#10902=CARTESIAN_POINT('Ctrl Pts',(1.10000067525152,1.22182202639256,0.664788091882127));
#10903=CARTESIAN_POINT('Ctrl Pts',(1.10000068775799,1.22694487635592,0.658801012170571));
#10904=CARTESIAN_POINT('Ctrl Pts',(1.10000222199399,1.23132099043293,0.652185071179834));
#10905=CARTESIAN_POINT('Ctrl Pts',(1.10000276904041,1.23488987417606,0.64510534613808));
#10906=CARTESIAN_POINT('Ctrl Pts',(1.10000282439334,1.23525099193115,0.644388983656765));
#10907=CARTESIAN_POINT('Ctrl Pts',(1.10000287212626,1.23560380546488,0.64366785367332));
#10908=CARTESIAN_POINT('Ctrl Pts',(1.10000291138002,1.23594822450451,0.642942116631622));
#10909=CARTESIAN_POINT('Ctrl Pts',(1.10000329911404,1.23935026814133,0.635773555081239));
#10910=CARTESIAN_POINT('Ctrl Pts',(1.10000258010782,1.24189771450306,0.628240464257889));
#10911=CARTESIAN_POINT('Ctrl Pts',(1.10000149084855,1.24353681278199,0.620511076118615));
#10912=CARTESIAN_POINT('Ctrl Pts',(1.10000079446814,1.24458471384188,0.615569557890241));
#10913=CARTESIAN_POINT('Ctrl Pts',(1.10000000111128,1.24526049271905,0.610547146027233));
#10914=CARTESIAN_POINT('Ctrl Pts',(1.09999999916631,1.24553911263843,0.605485603997432));
#10915=CARTESIAN_POINT('',(3.5,1.34358136363184,0.605270327458635));
#10916=CARTESIAN_POINT('Ctrl Pts',(3.5,1.34358136363184,0.605270327458635));
#10917=CARTESIAN_POINT('Ctrl Pts',(2.6995848679345,1.32722445934619,0.605308375488923));
#10918=CARTESIAN_POINT('Ctrl Pts',(1.89930203168261,1.29563783986497,0.605377360150118));
#10919=CARTESIAN_POINT('Ctrl Pts',(1.09999999916631,1.24553911263843,0.605485603997431));
#10920=CARTESIAN_POINT('',(3.5,1.24369946473792,0.7));
#10921=CARTESIAN_POINT('Ctrl Pts',(3.5,1.34358136363184,0.605270327458635));
#10922=CARTESIAN_POINT('Ctrl Pts',(3.5,1.34316359984937,0.613184373088104));
#10923=CARTESIAN_POINT('Ctrl Pts',(3.50000057901142,1.34177887744868,0.621008021569537));
#10924=CARTESIAN_POINT('Ctrl Pts',(3.50000082863025,1.33951086762262,0.628580534231506));
#10925=CARTESIAN_POINT('Ctrl Pts',(3.50000096811,1.33824356956914,0.632811834486987));
#10926=CARTESIAN_POINT('Ctrl Pts',(3.50000102536574,1.33669948631919,0.636964759527324));
#10927=CARTESIAN_POINT('Ctrl Pts',(3.50000098105742,1.334886463945,0.641009258704104));
#10928=CARTESIAN_POINT('Ctrl Pts',(3.50000090179773,1.3316432906201,0.648244145614236));
#10929=CARTESIAN_POINT('Ctrl Pts',(3.50000044940971,1.3275777080273,0.655054131048541));
#10930=CARTESIAN_POINT('Ctrl Pts',(3.50000027423476,1.32275302640998,0.661275670751788));
#10931=CARTESIAN_POINT('Ctrl Pts',(3.50000024156065,1.32185311357394,0.66243612938574));
#10932=CARTESIAN_POINT('Ctrl Pts',(3.50000022115524,1.32092666334894,0.663576045687695));
#10933=CARTESIAN_POINT('Ctrl Pts',(3.50000022069074,1.31997391848392,0.664694242102532));
#10934=CARTESIAN_POINT('Ctrl Pts',(3.50000021976176,1.31806844339147,0.666930617752677));
#10935=CARTESIAN_POINT('Ctrl Pts',(3.50000029790302,1.31605782519,0.669080165434128));
#10936=CARTESIAN_POINT('Ctrl Pts',(3.50000040488465,1.31394946763378,0.671139079687271));
#10937=CARTESIAN_POINT('Ctrl Pts',(3.50000069329649,1.3082655455861,0.6766897075128));
#10938=CARTESIAN_POINT('Ctrl Pts',(3.5000011432336,1.30193818666762,0.681521899278667));
#10939=CARTESIAN_POINT('Ctrl Pts',(3.50000129797765,1.29513115062548,0.68558123547136));
#10940=CARTESIAN_POINT('Ctrl Pts',(3.50000139624096,1.2908086457691,0.688158936000333));
#10941=CARTESIAN_POINT('Ctrl Pts',(3.50000139493488,1.28629176508013,0.690424313967808));
#10942=CARTESIAN_POINT('Ctrl Pts',(3.50000129141552,1.28161680488022,0.692354162840695));
#10943=CARTESIAN_POINT('Ctrl Pts',(3.50000112941005,1.27430059661786,0.695374333209024));
#10944=CARTESIAN_POINT('Ctrl Pts',(3.5000007162179,1.26668229982361,0.697540280949125));
#10945=CARTESIAN_POINT('Ctrl Pts',(3.50000038344698,1.25890895215876,0.698782355543395));
#10946=CARTESIAN_POINT('Ctrl Pts',(3.50000016866387,1.25389173534334,0.699584038140014));
#10947=CARTESIAN_POINT('Ctrl Pts',(3.4999999993056,1.24880933504677,0.69999999987784));
#10948=CARTESIAN_POINT('Ctrl Pts',(3.49999999991873,1.24369946470729,0.7));
#10949=CARTESIAN_POINT('Ctrl Pts',(2.80762377174497,1.22564400643366,0.7));
#10950=CARTESIAN_POINT('Ctrl Pts',(3.03837960601223,1.23298334400942,0.7));
#10951=CARTESIAN_POINT('Ctrl Pts',(3.26917843294065,1.23897560812206,0.7));
#10952=CARTESIAN_POINT('Ctrl Pts',(3.49999999991873,1.24369946470729,0.7));
#10953=CARTESIAN_POINT('Ctrl Pts',(7.29709043526678,1.22049830417059,0.7));
#10954=CARTESIAN_POINT('Ctrl Pts',(8.19846709497879,1.19422430779862,0.7));
#10955=CARTESIAN_POINT('Ctrl Pts',(9.09944331332256,1.15544418981837,0.7));
#10956=CARTESIAN_POINT('Ctrl Pts',(10.,1.10900986674273,0.7));
#10957=CARTESIAN_POINT('Ctrl Pts',(7.29793284700474,1.24939875264889,0.7));
#10958=CARTESIAN_POINT('Ctrl Pts',(8.19957769811722,1.22310890030201,0.699999704549177));
#10959=CARTESIAN_POINT('Ctrl Pts',(9.10076698492607,1.18430758604571,0.700000491839571));
#10960=CARTESIAN_POINT('Ctrl Pts',(10.0014871213396,1.13785139984992,0.7));
#10961=CARTESIAN_POINT('Ctrl Pts',(7.29939288958794,1.29948813715084,0.676630595533454));
#10962=CARTESIAN_POINT('Ctrl Pts',(8.20149954052228,1.27317186922949,0.676644146017132));
#10963=CARTESIAN_POINT('Ctrl Pts',(9.10306300621911,1.23433322993607,0.676664155483857));
#10964=CARTESIAN_POINT('Ctrl Pts',(10.0040646682326,1.18784086746588,0.676686753673613));
#10965=CARTESIAN_POINT('Ctrl Pts',(7.29996660609513,1.31917051289423,0.626939603849942));
#10966=CARTESIAN_POINT('Ctrl Pts',(8.20225661204673,1.29285896783792,0.626974637782525));
#10967=CARTESIAN_POINT('Ctrl Pts',(9.10396596140606,1.25402923300358,0.627026849623412));
#10968=CARTESIAN_POINT('Ctrl Pts',(10.0050807923581,1.20754778500352,0.627085325222079));
#10969=CARTESIAN_POINT('Ctrl Pts',(7.29999999953093,1.32031613471704,0.605285370449856));
#10970=CARTESIAN_POINT('Ctrl Pts',(8.20230020786565,1.29401302889245,0.605326714446839));
#10971=CARTESIAN_POINT('Ctrl Pts',(9.10401978846669,1.25519559703033,0.605388684776982));
#10972=CARTESIAN_POINT('Ctrl Pts',(10.0051416645797,1.20872835322339,0.605457722909465));
#10973=CARTESIAN_POINT('',(7.29999999989017,1.22041345054104,0.7));
#10974=CARTESIAN_POINT('Ctrl Pts',(7.29999999978094,1.22041345055303,0.7));
#10975=CARTESIAN_POINT('Ctrl Pts',(7.51641201913776,1.21409884615949,0.7));
#10976=CARTESIAN_POINT('Ctrl Pts',(7.73280095443524,1.20706364503479,0.7));
#10977=CARTESIAN_POINT('Ctrl Pts',(7.94916654146952,1.19937499621344,0.7));
#10978=CARTESIAN_POINT('',(7.29999999953133,1.3203161347307,0.605285370449834));
#10979=CARTESIAN_POINT('Ctrl Pts',(7.29999999989087,1.22041345054982,0.7));
#10980=CARTESIAN_POINT('Ctrl Pts',(7.30000000079355,1.22832360919786,0.699999999740221));
#10981=CARTESIAN_POINT('Ctrl Pts',(7.29999941101664,1.23617007614594,0.699006006469939));
#10982=CARTESIAN_POINT('Ctrl Pts',(7.29999889581476,1.24381267896118,0.697118889344366));
#10983=CARTESIAN_POINT('Ctrl Pts',(7.29999860583198,1.24811433880851,0.696056720321257));
#10984=CARTESIAN_POINT('Ctrl Pts',(7.29999834128398,1.25235147078274,0.694710570513598));
#10985=CARTESIAN_POINT('Ctrl Pts',(7.29999817264931,1.25649739217805,0.693091458416622));
#10986=CARTESIAN_POINT('Ctrl Pts',(7.29999787070862,1.26392067210813,0.690192435210923));
#10987=CARTESIAN_POINT('Ctrl Pts',(7.29999793286912,1.27097116792553,0.686452948287278));
#10988=CARTESIAN_POINT('Ctrl Pts',(7.2999983123982,1.27750284616821,0.681954753865011));
#10989=CARTESIAN_POINT('Ctrl Pts',(7.2999985213788,1.28109939299731,0.679477906983553));
#10990=CARTESIAN_POINT('Ctrl Pts',(7.29999881895966,1.28453837241868,0.676770138671336));
#10991=CARTESIAN_POINT('Ctrl Pts',(7.29999908362886,1.28779148632494,0.673839551409954));
#10992=CARTESIAN_POINT('Ctrl Pts',(7.29999934163235,1.29096267037196,0.670982771155867));
#10993=CARTESIAN_POINT('Ctrl Pts',(7.29999957112158,1.2939379836903,0.667931525418885));
#10994=CARTESIAN_POINT('Ctrl Pts',(7.29999957127586,1.29669488996436,0.664697318929259));
#10995=CARTESIAN_POINT('Ctrl Pts',(7.29999957156178,1.30180432468448,0.658703293276094));
#10996=CARTESIAN_POINT('Ctrl Pts',(7.29999886995656,1.30616650855536,0.652082235935803));
#10997=CARTESIAN_POINT('Ctrl Pts',(7.29999863193158,1.30972187224872,0.644999691185358));
#10998=CARTESIAN_POINT('Ctrl Pts',(7.29999860759325,1.31008541227461,0.644275492840527));
#10999=CARTESIAN_POINT('Ctrl Pts',(7.29999858692673,1.31044047656777,0.643546449710686));
#11000=CARTESIAN_POINT('Ctrl Pts',(7.29999857034625,1.31078697300061,0.642812727646596));
#11001=CARTESIAN_POINT('Ctrl Pts',(7.29999840819729,1.31417553742296,0.635637287305567));
#11002=CARTESIAN_POINT('Ctrl Pts',(7.29999876577208,1.31670951795567,0.628098908385918));
#11003=CARTESIAN_POINT('Ctrl Pts',(7.29999928780719,1.3183355664444,0.620365998324013));
#11004=CARTESIAN_POINT('Ctrl Pts',(7.29999962266353,1.3193785856694,0.615405768714856));
#11005=CARTESIAN_POINT('Ctrl Pts',(7.3,1.32004717656055,0.610364828659741));
#11006=CARTESIAN_POINT('Ctrl Pts',(7.3,1.32031613470337,0.605285370449877));
#11007=CARTESIAN_POINT('',(10.,1.20899340483173,0.605457329065657));
#11008=CARTESIAN_POINT('Ctrl Pts',(9.99999999968202,1.20899340489109,0.605457329065633));
#11009=CARTESIAN_POINT('Ctrl Pts',(9.10058974048747,1.25534320916473,0.605388449123016));
#11010=CARTESIAN_POINT('Ctrl Pts',(8.20058408060299,1.29406305600824,0.605326635812744));
#11011=CARTESIAN_POINT('Ctrl Pts',(7.29999999953093,1.32031613471704,0.605285370449856));
#11012=CARTESIAN_POINT('',(9.99999999523418,1.1090098672342,0.7));
#11013=CARTESIAN_POINT('Ctrl Pts',(9.99999999968202,1.20899340489109,0.605457329065633));
#11014=CARTESIAN_POINT('Ctrl Pts',(9.99999999887489,1.20856043137698,0.613368813757176));
#11015=CARTESIAN_POINT('Ctrl Pts',(9.99999852309337,1.20715974444566,0.621187403383205));
#11016=CARTESIAN_POINT('Ctrl Pts',(9.99999786661901,1.20487567413208,0.628752957409046));
#11017=CARTESIAN_POINT('Ctrl Pts',(9.9999975031266,1.20361097553651,0.63294203403));
#11018=CARTESIAN_POINT('Ctrl Pts',(9.99999733971606,1.20207445367248,0.63705356322819));
#11019=CARTESIAN_POINT('Ctrl Pts',(9.99999742766416,1.20027388348257,0.64105842070465));
#11020=CARTESIAN_POINT('Ctrl Pts',(9.9999975865154,1.19702170610966,0.6482919664668));
#11021=CARTESIAN_POINT('Ctrl Pts',(9.99999868569093,1.19294650045069,0.655099368158521));
#11022=CARTESIAN_POINT('Ctrl Pts',(9.9999991134218,1.18811276085989,0.661317774786376));
#11023=CARTESIAN_POINT('Ctrl Pts',(9.99999919410111,1.18720101282252,0.662490701033652));
#11024=CARTESIAN_POINT('Ctrl Pts',(9.99999924414009,1.18626214680169,0.663642601192937));
#11025=CARTESIAN_POINT('Ctrl Pts',(9.99999924372355,1.18529642131707,0.664772262763739));
#11026=CARTESIAN_POINT('Ctrl Pts',(9.99999924291654,1.18342543943696,0.666960851926287));
#11027=CARTESIAN_POINT('Ctrl Pts',(9.99999905429896,1.18145367213587,0.669066014649603));
#11028=CARTESIAN_POINT('Ctrl Pts',(9.99999879621773,1.17938809187152,0.671084194359814));
#11029=CARTESIAN_POINT('Ctrl Pts',(9.99999808597787,1.17370361260899,0.676638227242868));
#11030=CARTESIAN_POINT('Ctrl Pts',(9.9999969699445,1.16737553754052,0.681473799108647));
#11031=CARTESIAN_POINT('Ctrl Pts',(9.99999660204079,1.16056788011185,0.685537070165577));
#11032=CARTESIAN_POINT('Ctrl Pts',(9.99999636768906,1.15623145667386,0.688125341392612));
#11033=CARTESIAN_POINT('Ctrl Pts',(9.99999638726733,1.15169947441128,0.690399565850749));
#11034=CARTESIAN_POINT('Ctrl Pts',(9.99999666360534,1.14700857532255,0.692336497939236));
#11035=CARTESIAN_POINT('Ctrl Pts',(9.99999709503399,1.13968497812548,0.695360504669253));
#11036=CARTESIAN_POINT('Ctrl Pts',(9.99999815490668,1.13205884654683,0.697530003145419));
#11037=CARTESIAN_POINT('Ctrl Pts',(9.99999900983214,1.12427739544825,0.698775573347137));
#11038=CARTESIAN_POINT('Ctrl Pts',(9.99999956314479,1.11924119569193,0.699581713521624));
#11039=CARTESIAN_POINT('Ctrl Pts',(10.,1.11413933950174,0.7));
#11040=CARTESIAN_POINT('Ctrl Pts',(10.,1.10900986674273,0.7));
#11041=CARTESIAN_POINT('Ctrl Pts',(8.26514054272776,1.18768929227839,0.7));
#11042=CARTESIAN_POINT('Ctrl Pts',(8.84359655063997,1.16547286645366,0.7));
#11043=CARTESIAN_POINT('Ctrl Pts',(9.42188471826001,1.13881853081542,0.7));
#11044=CARTESIAN_POINT('Ctrl Pts',(9.99999999522154,1.10900986698912,0.7));
#11045=CARTESIAN_POINT('Origin',(5.4,-8.11656130105013E-18,0.7));
#11046=CARTESIAN_POINT('',(7.3,-1.22041345053557,0.7));
#11047=CARTESIAN_POINT('Ctrl Pts',(7.94916654049851,-1.19937499624794,0.7));
#11048=CARTESIAN_POINT('Ctrl Pts',(7.73280095382446,-1.20706364505454,0.7));
#11049=CARTESIAN_POINT('Ctrl Pts',(7.51641201888728,-1.21409884616656,0.7));
#11050=CARTESIAN_POINT('Ctrl Pts',(7.29999999989085,-1.22041345054982,0.7));
#11051=CARTESIAN_POINT('',(7.3,-0.712777777777778,0.7));
#11052=CARTESIAN_POINT('',(10.,-1.10900986674244,0.7));
#11053=CARTESIAN_POINT('',(10.,0.653773457742722,0.7));
#11054=CARTESIAN_POINT('Ctrl Pts',(10.,-1.10900986674273,0.7));
#11055=CARTESIAN_POINT('Ctrl Pts',(9.42188472144661,-1.13881853066854,0.7));
#11056=CARTESIAN_POINT('Ctrl Pts',(8.84359655223373,-1.16547286639245,0.7));
#11057=CARTESIAN_POINT('Ctrl Pts',(8.26514054272776,-1.18768929227839,0.7));
#11058=CARTESIAN_POINT('',(7.95,-1.,0.7));
#11059=CARTESIAN_POINT('Origin',(8.1,-1.,0.7));
#11060=CARTESIAN_POINT('',(7.95,1.,0.7));
#11061=CARTESIAN_POINT('Origin',(8.1,1.,0.7));
#11062=CARTESIAN_POINT('',(8.4,-4.89858719658942E-17,0.7));
#11063=CARTESIAN_POINT('Origin',(8.8,0.,0.7));
#11064=CARTESIAN_POINT('Origin',(8.97320508075689,0.3,0.9));
#11065=CARTESIAN_POINT('',(8.97320508075689,0.3,0.9));
#11066=CARTESIAN_POINT('',(9.14641016151377,0.,0.9));
#11067=CARTESIAN_POINT('',(8.59150635094611,0.961121593216771,0.9));
#11068=CARTESIAN_POINT('',(8.97320508075689,0.3,0.6));
#11069=CARTESIAN_POINT('',(8.97320508075689,0.3,0.9));
#11070=CARTESIAN_POINT('',(9.14641016151377,0.,0.6));
#11071=CARTESIAN_POINT('',(9.14641016151377,0.,0.6));
#11072=CARTESIAN_POINT('',(9.14641016151377,0.,0.9));
#11073=CARTESIAN_POINT('Origin',(8.62679491924311,0.3,0.9));
#11074=CARTESIAN_POINT('',(8.62679491924311,0.3,0.9));
#11075=CARTESIAN_POINT('',(7.01339745962156,0.3,0.9));
#11076=CARTESIAN_POINT('',(8.62679491924311,0.3,0.6));
#11077=CARTESIAN_POINT('',(8.62679491924311,0.3,0.9));
#11078=CARTESIAN_POINT('',(8.97320508075689,0.3,0.6));
#11079=CARTESIAN_POINT('Origin',(8.45358983848623,5.55111512312578E-17,
0.9));
#11080=CARTESIAN_POINT('',(8.45358983848623,4.24230095489963E-17,0.9));
#11081=CARTESIAN_POINT('',(8.07189110867545,-0.661121593216771,0.9));
#11082=CARTESIAN_POINT('',(8.45358983848623,5.55111512312578E-17,0.6));
#11083=CARTESIAN_POINT('',(8.45358983848623,4.24230095489963E-17,0.9));
#11084=CARTESIAN_POINT('',(8.62679491924311,0.3,0.6));
#11085=CARTESIAN_POINT('Origin',(8.62679491924311,-0.3,0.9));
#11086=CARTESIAN_POINT('',(8.62679491924311,-0.3,0.9));
#11087=CARTESIAN_POINT('',(8.15849364905389,0.511121593216771,0.9));
#11088=CARTESIAN_POINT('',(8.62679491924311,-0.3,0.6));
#11089=CARTESIAN_POINT('',(8.62679491924311,-0.3,0.9));
#11090=CARTESIAN_POINT('',(8.45358983848623,4.24230095489963E-17,0.6));
#11091=CARTESIAN_POINT('Origin',(8.97320508075689,-0.3,0.9));
#11092=CARTESIAN_POINT('',(8.97320508075689,-0.3,0.9));
#11093=CARTESIAN_POINT('',(7.18660254037844,-0.3,0.9));
#11094=CARTESIAN_POINT('',(8.97320508075689,-0.3,0.6));
#11095=CARTESIAN_POINT('',(8.97320508075689,-0.3,0.9));
#11096=CARTESIAN_POINT('',(8.62679491924311,-0.3,0.6));
#11097=CARTESIAN_POINT('Origin',(9.14641016151377,0.,0.9));
#11098=CARTESIAN_POINT('',(8.67810889132456,-0.811121593216771,0.9));
#11099=CARTESIAN_POINT('',(8.97320508075689,-0.3,0.6));
#11100=CARTESIAN_POINT('Origin',(8.8,5.55111512312578E-17,0.6));
#11101=CARTESIAN_POINT('',(8.63,-2.0818995585505E-17,0.6));
#11102=CARTESIAN_POINT('Origin',(8.8,0.,0.6));
#11103=CARTESIAN_POINT('Origin',(2.17320508075689,0.3,0.9));
#11104=CARTESIAN_POINT('',(2.17320508075689,0.3,0.9));
#11105=CARTESIAN_POINT('',(2.34641016151378,0.,0.9));
#11106=CARTESIAN_POINT('',(2.64150635094611,-0.511121593216773,0.9));
#11107=CARTESIAN_POINT('',(2.17320508075689,0.3,0.6));
#11108=CARTESIAN_POINT('',(2.17320508075689,0.3,0.9));
#11109=CARTESIAN_POINT('',(2.34641016151378,0.,0.6));
#11110=CARTESIAN_POINT('',(2.34641016151378,0.,0.6));
#11111=CARTESIAN_POINT('',(2.34641016151378,0.,0.9));
#11112=CARTESIAN_POINT('Origin',(1.82679491924311,0.3,0.9));
#11113=CARTESIAN_POINT('',(1.82679491924311,0.3,0.9));
#11114=CARTESIAN_POINT('',(3.61339745962156,0.3,0.9));
#11115=CARTESIAN_POINT('',(1.82679491924311,0.3,0.6));
#11116=CARTESIAN_POINT('',(1.82679491924311,0.3,0.9));
#11117=CARTESIAN_POINT('',(2.17320508075689,0.3,0.6));
#11118=CARTESIAN_POINT('Origin',(1.65358983848622,5.55111512312578E-17,
0.9));
#11119=CARTESIAN_POINT('',(1.65358983848622,4.24230095489963E-17,0.9));
#11120=CARTESIAN_POINT('',(2.12189110867545,0.811121593216773,0.9));
#11121=CARTESIAN_POINT('',(1.65358983848622,5.55111512312578E-17,0.6));
#11122=CARTESIAN_POINT('',(1.65358983848622,4.24230095489963E-17,0.9));
#11123=CARTESIAN_POINT('',(1.82679491924311,0.3,0.6));
#11124=CARTESIAN_POINT('Origin',(1.82679491924311,-0.3,0.9));
#11125=CARTESIAN_POINT('',(1.82679491924311,-0.3,0.9));
#11126=CARTESIAN_POINT('',(2.20849364905389,-0.961121593216772,0.9));
#11127=CARTESIAN_POINT('',(1.82679491924311,-0.3,0.6));
#11128=CARTESIAN_POINT('',(1.82679491924311,-0.3,0.9));
#11129=CARTESIAN_POINT('',(1.65358983848622,4.24230095489963E-17,0.6));
#11130=CARTESIAN_POINT('Origin',(2.17320508075689,-0.3,0.9));
#11131=CARTESIAN_POINT('',(2.17320508075689,-0.3,0.9));
#11132=CARTESIAN_POINT('',(3.78660254037844,-0.3,0.9));
#11133=CARTESIAN_POINT('',(2.17320508075689,-0.3,0.6));
#11134=CARTESIAN_POINT('',(2.17320508075689,-0.3,0.9));
#11135=CARTESIAN_POINT('',(1.82679491924311,-0.3,0.6));
#11136=CARTESIAN_POINT('Origin',(2.34641016151378,0.,0.9));
#11137=CARTESIAN_POINT('',(2.72810889132455,0.661121593216773,0.9));
#11138=CARTESIAN_POINT('',(2.17320508075689,-0.3,0.6));
#11139=CARTESIAN_POINT('Origin',(2.,5.55111512312578E-17,0.6));
#11140=CARTESIAN_POINT('',(1.83,-2.0818995585505E-17,0.6));
#11141=CARTESIAN_POINT('Origin',(2.,0.,0.6));
#11142=CARTESIAN_POINT('Origin',(8.1,-1.,0.8));
#11143=CARTESIAN_POINT('',(7.95,-1.,0.9));
#11144=CARTESIAN_POINT('Origin',(8.1,-1.,0.9));
#11145=CARTESIAN_POINT('',(7.95,-1.,0.8));
#11146=CARTESIAN_POINT('Origin',(2.7,-1.,0.8));
#11147=CARTESIAN_POINT('',(2.55,-1.,0.9));
#11148=CARTESIAN_POINT('Origin',(2.7,-1.,0.9));
#11149=CARTESIAN_POINT('',(2.55,-1.,0.7));
#11150=CARTESIAN_POINT('',(2.55,-1.,0.8));
#11151=CARTESIAN_POINT('Origin',(2.7,-1.,0.7));
#11152=CARTESIAN_POINT('Origin',(2.7,1.,0.8));
#11153=CARTESIAN_POINT('',(2.55,1.,0.9));
#11154=CARTESIAN_POINT('Origin',(2.7,1.,0.9));
#11155=CARTESIAN_POINT('',(2.55,1.,0.7));
#11156=CARTESIAN_POINT('',(2.55,1.,0.8));
#11157=CARTESIAN_POINT('Origin',(2.7,1.,0.7));
#11158=CARTESIAN_POINT('Origin',(8.1,1.,0.8));
#11159=CARTESIAN_POINT('',(7.95,1.,0.9));
#11160=CARTESIAN_POINT('Origin',(8.1,1.,0.9));
#11161=CARTESIAN_POINT('',(7.95,1.,0.8));
#11162=CARTESIAN_POINT('Origin',(2.,0.,0.45));
#11163=CARTESIAN_POINT('',(1.83,-2.0818995585505E-17,0.32));
#11164=CARTESIAN_POINT('',(1.83,2.0818995585505E-17,0.45));
#11165=CARTESIAN_POINT('Origin',(2.,0.,0.32));
#11166=CARTESIAN_POINT('Origin',(8.8,0.,0.45));
#11167=CARTESIAN_POINT('',(8.63,-2.0818995585505E-17,0.32));
#11168=CARTESIAN_POINT('',(8.63,2.0818995585505E-17,0.45));
#11169=CARTESIAN_POINT('Origin',(8.8,0.,0.32));
#11170=CARTESIAN_POINT('Origin',(10.,-0.62,0.32));
#11171=CARTESIAN_POINT('',(0.200274469199584,-0.62,0.));
#11172=CARTESIAN_POINT('',(0.217044958570157,-0.62,0.32));
#11173=CARTESIAN_POINT('',(0.221783445591644,-0.62,0.410415718550007));
#11174=CARTESIAN_POINT('',(0.,-0.62,0.));
#11175=CARTESIAN_POINT('',(7.7,-0.62,0.));
#11176=CARTESIAN_POINT('',(0.0167704893705732,-0.62,0.32));
#11177=CARTESIAN_POINT('',(0.0220575386407278,-0.62,0.420882909798596));
#11178=CARTESIAN_POINT('',(-0.1,-0.62,0.32));
#11179=CARTESIAN_POINT('Origin',(10.,-0.62,0.32));
#11180=CARTESIAN_POINT('',(0.9,-0.62,0.32));
#11181=CARTESIAN_POINT('',(0.9,-0.62,0.));
#11182=CARTESIAN_POINT('',(0.9,-0.62,0.16));
#11183=CARTESIAN_POINT('',(1.1,-0.62,0.32));
#11184=CARTESIAN_POINT('',(-0.1,-0.62,0.32));
#11185=CARTESIAN_POINT('',(1.1,-0.62,0.));
#11186=CARTESIAN_POINT('',(1.1,-0.62,0.16));
#11187=CARTESIAN_POINT('',(7.7,-0.62,0.));
#11188=CARTESIAN_POINT('Origin',(10.,-0.62,0.32));
#11189=CARTESIAN_POINT('',(3.5,-0.62,0.32));
#11190=CARTESIAN_POINT('',(3.5,-0.62,0.));
#11191=CARTESIAN_POINT('',(3.5,-0.62,0.16));
#11192=CARTESIAN_POINT('',(3.7,-0.62,0.32));
#11193=CARTESIAN_POINT('',(-0.1,-0.62,0.32));
#11194=CARTESIAN_POINT('',(3.7,-0.62,0.));
#11195=CARTESIAN_POINT('',(3.7,-0.62,0.16));
#11196=CARTESIAN_POINT('',(7.7,-0.62,0.));
#11197=CARTESIAN_POINT('Origin',(10.,-0.62,0.32));
#11198=CARTESIAN_POINT('',(7.1,-0.62,0.32));
#11199=CARTESIAN_POINT('',(7.1,-0.62,0.));
#11200=CARTESIAN_POINT('',(7.1,-0.62,0.16));
#11201=CARTESIAN_POINT('',(7.3,-0.62,0.32));
#11202=CARTESIAN_POINT('',(-0.1,-0.62,0.32));
#11203=CARTESIAN_POINT('',(7.3,-0.62,0.));
#11204=CARTESIAN_POINT('',(7.3,-0.62,0.16));
#11205=CARTESIAN_POINT('',(7.7,-0.62,0.));
#11206=CARTESIAN_POINT('Origin',(-0.0999999999999996,0.62,0.32));
#11207=CARTESIAN_POINT('',(0.217044958570158,0.62,0.32));
#11208=CARTESIAN_POINT('',(0.200274469199584,0.62,0.));
#11209=CARTESIAN_POINT('',(0.207951231396534,0.62,0.146481348799182));
#11210=CARTESIAN_POINT('',(0.0167704893705736,0.62,0.32));
#11211=CARTESIAN_POINT('',(10.,0.62,0.32));
#11212=CARTESIAN_POINT('',(0.,0.62,0.));
#11213=CARTESIAN_POINT('',(0.00822532444561912,0.62,0.156948540047771));
#11214=CARTESIAN_POINT('',(2.65,0.62,0.));
#11215=CARTESIAN_POINT('Origin',(-0.0999999999999996,0.62,0.32));
#11216=CARTESIAN_POINT('',(0.9,0.62,0.));
#11217=CARTESIAN_POINT('',(0.9,0.62,0.32));
#11218=CARTESIAN_POINT('',(0.9,0.62,0.16));
#11219=CARTESIAN_POINT('',(1.1,0.62,0.));
#11220=CARTESIAN_POINT('',(2.65,0.62,0.));
#11221=CARTESIAN_POINT('',(1.1,0.62,0.32));
#11222=CARTESIAN_POINT('',(1.1,0.62,0.16));
#11223=CARTESIAN_POINT('',(10.,0.62,0.32));
#11224=CARTESIAN_POINT('Origin',(-0.0999999999999996,0.62,0.32));
#11225=CARTESIAN_POINT('',(3.5,0.62,0.));
#11226=CARTESIAN_POINT('',(3.5,0.62,0.32));
#11227=CARTESIAN_POINT('',(3.5,0.62,0.16));
#11228=CARTESIAN_POINT('',(3.7,0.62,0.));
#11229=CARTESIAN_POINT('',(2.65,0.62,0.));
#11230=CARTESIAN_POINT('',(3.7,0.62,0.32));
#11231=CARTESIAN_POINT('',(3.7,0.62,0.16));
#11232=CARTESIAN_POINT('',(10.,0.62,0.32));
#11233=CARTESIAN_POINT('Origin',(4.95,0.,0.32));
#11234=CARTESIAN_POINT('',(1.6,-4.89858719658941E-17,0.32));
#11235=CARTESIAN_POINT('Origin',(2.,0.,0.32));
#11236=CARTESIAN_POINT('Origin',(4.95,0.,0.32));
#11237=CARTESIAN_POINT('',(8.4,-4.89858719658942E-17,0.32));
#11238=CARTESIAN_POINT('Origin',(8.8,0.,0.32));
#11239=CARTESIAN_POINT('Origin',(4.95,0.,0.32));
#11240=CARTESIAN_POINT('',(0.217044958570157,-0.7,0.32));
#11241=CARTESIAN_POINT('',(0.0167704893705731,-0.7,0.32));
#11242=CARTESIAN_POINT('Origin',(4.95,0.,0.32));
#11243=CARTESIAN_POINT('',(0.9,0.671641708581009,0.32));
#11244=CARTESIAN_POINT('',(1.1,-0.671641708581009,0.32));
#11245=CARTESIAN_POINT('Origin',(4.95,0.,0.32));
#11246=CARTESIAN_POINT('',(3.5,0.723888888888889,0.32));
#11247=CARTESIAN_POINT('',(3.7,-0.723888888888889,0.32));
#11248=CARTESIAN_POINT('Origin',(4.95,0.,0.32));
#11249=CARTESIAN_POINT('',(7.1,0.62,0.32));
#11250=CARTESIAN_POINT('',(7.1,0.712777777777778,0.32));
#11251=CARTESIAN_POINT('',(7.3,0.62,0.32));
#11252=CARTESIAN_POINT('',(10.,0.62,0.32));
#11253=CARTESIAN_POINT('',(7.3,-0.712777777777778,0.32));
#11254=CARTESIAN_POINT('Origin',(-0.0999999999999996,0.62,0.32));
#11255=CARTESIAN_POINT('',(7.1,0.62,0.));
#11256=CARTESIAN_POINT('',(7.1,0.62,0.16));
#11257=CARTESIAN_POINT('',(7.3,0.62,0.));
#11258=CARTESIAN_POINT('',(2.65,0.62,0.));
#11259=CARTESIAN_POINT('',(7.3,0.62,0.16));
#11260=CARTESIAN_POINT('Origin',(10.,1.30754691548544,0.));
#11261=CARTESIAN_POINT('',(10.,1.24211782565704,0.));
#11262=CARTESIAN_POINT('',(10.,-1.24211782565704,0.));
#11263=CARTESIAN_POINT('',(10.,1.30754691548544,0.));
#11264=CARTESIAN_POINT('',(10.,-1.20899340483173,0.605457329065657));
#11265=CARTESIAN_POINT('Ctrl Pts',(10.,-1.20899340483173,0.605457329065657));
#11266=CARTESIAN_POINT('Ctrl Pts',(10.,-1.21451837038612,0.504502771559899));
#11267=CARTESIAN_POINT('Ctrl Pts',(10.,-1.22004249263249,0.403547366186347));
#11268=CARTESIAN_POINT('Ctrl Pts',(10.,-1.23108392958594,0.201728789021226));
#11269=CARTESIAN_POINT('Ctrl Pts',(10.,-1.23660133320922,0.100864020914724));
#11270=CARTESIAN_POINT('Ctrl Pts',(10.,-1.24211782565704,0.));
#11271=CARTESIAN_POINT('Ctrl Pts',(10.,-1.10900986674273,0.7));
#11272=CARTESIAN_POINT('Ctrl Pts',(10.,-1.11692706738765,0.7));
#11273=CARTESIAN_POINT('Ctrl Pts',(9.99999896020971,-1.12478097169818,0.699006158364426));
#11274=CARTESIAN_POINT('Ctrl Pts',(9.99999805494427,-1.13243115645175,0.697118998397561));
#11275=CARTESIAN_POINT('Ctrl Pts',(9.99999754769332,-1.13671781459207,0.696061558623929));
#11276=CARTESIAN_POINT('Ctrl Pts',(9.99999708556116,-1.14094056283945,0.694722610426682));
#11277=CARTESIAN_POINT('Ctrl Pts',(9.99999679002998,-1.14507302265453,0.693112977943955));
#11278=CARTESIAN_POINT('Ctrl Pts',(9.99999625879002,-1.15250143622127,0.690219540062595));
#11279=CARTESIAN_POINT('Ctrl Pts',(9.999996365957,-1.15955821040664,0.686485807665162));
#11280=CARTESIAN_POINT('Ctrl Pts',(9.99999703387985,-1.16609707610076,0.681992895329386));
#11281=CARTESIAN_POINT('Ctrl Pts',(9.99999740034986,-1.16968476316425,0.679527763880215));
#11282=CARTESIAN_POINT('Ctrl Pts',(9.99999792190556,-1.17311627083768,0.676833210412541));
#11283=CARTESIAN_POINT('Ctrl Pts',(9.99999838578331,-1.17636354905877,0.673917165661822));
#11284=CARTESIAN_POINT('Ctrl Pts',(9.99999884023993,-1.17954487655573,0.671060344436104));
#11285=CARTESIAN_POINT('Ctrl Pts',(9.99999924462882,-1.18253006594632,0.668008218820746));
#11286=CARTESIAN_POINT('Ctrl Pts',(9.99999924442301,-1.185296421281,0.664772262763763));
#11287=CARTESIAN_POINT('Ctrl Pts',(9.99999924404215,-1.19041578560695,0.658783864313737));
#11288=CARTESIAN_POINT('Ctrl Pts',(9.99999800949836,-1.19478865237554,0.652167294255586));
#11289=CARTESIAN_POINT('Ctrl Pts',(9.99999759228052,-1.19835462180986,0.645087621913151));
#11290=CARTESIAN_POINT('Ctrl Pts',(9.99999755030119,-1.19871341999785,0.644375284453517));
#11291=CARTESIAN_POINT('Ctrl Pts',(9.9999975145836,-1.19906401030029,0.643658239626438));
#11292=CARTESIAN_POINT('Ctrl Pts',(9.99999748581823,-1.19940630408966,0.642936645100882));
#11293=CARTESIAN_POINT('Ctrl Pts',(9.99999720003888,-1.20280693749908,0.635767720253638));
#11294=CARTESIAN_POINT('Ctrl Pts',(9.9999978299417,-1.20535324884233,0.628234501710241));
#11295=CARTESIAN_POINT('Ctrl Pts',(9.99999874867777,-1.20699142055415,0.62050509267719));
#11296=CARTESIAN_POINT('Ctrl Pts',(9.99999933690345,-1.20804026874419,0.615556297251186));
#11297=CARTESIAN_POINT('Ctrl Pts',(9.99999999916487,-1.20871598809812,0.61052641213707));
#11298=CARTESIAN_POINT('Ctrl Pts',(9.99999999968202,-1.20899340489109,0.605457329065633));
#11299=CARTESIAN_POINT('Ctrl Pts',(10.,1.24211782565704,0.));
#11300=CARTESIAN_POINT('Ctrl Pts',(10.,1.23660053043673,0.100878698875723));
#11301=CARTESIAN_POINT('Ctrl Pts',(10.,1.23108232376984,0.201758145268796));
#11302=CARTESIAN_POINT('Ctrl Pts',(10.,1.22004088630648,0.403576722396156));
#11303=CARTESIAN_POINT('Ctrl Pts',(10.,1.2145175671044,0.504517449470448));
#11304=CARTESIAN_POINT('Ctrl Pts',(10.,1.20899340483173,0.605457329065657));
#11305=CARTESIAN_POINT('Origin',(7.3,-1.42555555555556,0.));
#11306=CARTESIAN_POINT('',(7.3,1.35236351479115,0.));
#11307=CARTESIAN_POINT('',(7.3,-1.42555555555556,0.));
#11308=CARTESIAN_POINT('Ctrl Pts',(7.29999999953133,1.3203161347307,0.605285370449834));
#11309=CARTESIAN_POINT('Ctrl Pts',(7.29999999953133,1.32565322760551,0.504490726585133));
#11310=CARTESIAN_POINT('Ctrl Pts',(7.3,1.33099015509697,0.403695123734478));
#11311=CARTESIAN_POINT('Ctrl Pts',(7.3,1.34167258064689,0.201933969199042));
#11312=CARTESIAN_POINT('Ctrl Pts',(7.3,1.34701817868136,0.100966514951419));
#11313=CARTESIAN_POINT('Ctrl Pts',(7.3,1.35236351479115,0.));
#11314=CARTESIAN_POINT('',(7.29999999953133,-1.3203161347307,0.605285370449834));
#11315=CARTESIAN_POINT('Ctrl Pts',(7.3,-1.32031613470337,0.605285370449877));
#11316=CARTESIAN_POINT('Ctrl Pts',(7.3,-1.31989712778929,0.61319860217968));
#11317=CARTESIAN_POINT('Ctrl Pts',(7.29999916171872,-1.31851071739963,0.621020829077898));
#11318=CARTESIAN_POINT('Ctrl Pts',(7.29999878808195,-1.31624092632926,0.628591660945423));
#11319=CARTESIAN_POINT('Ctrl Pts',(7.29999857947278,-1.31497365483497,0.632818613610392));
#11320=CARTESIAN_POINT('Ctrl Pts',(7.29999848639856,-1.31343001415,0.636967235874856));
#11321=CARTESIAN_POINT('Ctrl Pts',(7.29999853830689,-1.31161789606625,0.641007613679984));
#11322=CARTESIAN_POINT('Ctrl Pts',(7.29999863125487,-1.30837308502546,0.648242386418365));
#11323=CARTESIAN_POINT('Ctrl Pts',(7.29999925734287,-1.30430566789097,0.655052076019481));
#11324=CARTESIAN_POINT('Ctrl Pts',(7.29999949821933,-1.29947941328181,0.661273460789274));
#11325=CARTESIAN_POINT('Ctrl Pts',(7.29999954322,-1.29857776968225,0.662435743389828));
#11326=CARTESIAN_POINT('Ctrl Pts',(7.29999957102613,-1.29764951297213,0.663577423078133));
#11327=CARTESIAN_POINT('Ctrl Pts',(7.2999995707084,-1.29669488998092,0.664697318929248));
#11328=CARTESIAN_POINT('Ctrl Pts',(7.29999957007561,-1.29479368240016,0.666927680549918));
#11329=CARTESIAN_POINT('Ctrl Pts',(7.29999945886743,-1.29278792931167,0.669071688571899));
#11330=CARTESIAN_POINT('Ctrl Pts',(7.29999930790078,-1.2906849717248,0.671125563583336));
#11331=CARTESIAN_POINT('Ctrl Pts',(7.29999889984047,-1.28500071247856,0.676677153447665));
#11332=CARTESIAN_POINT('Ctrl Pts',(7.29999826931494,-1.27867319504519,0.681510485910933));
#11333=CARTESIAN_POINT('Ctrl Pts',(7.29999806345125,-1.27186607945067,0.685571085769401));
#11334=CARTESIAN_POINT('Ctrl Pts',(7.29999793266427,-1.26754145993833,0.688150820039508));
#11335=CARTESIAN_POINT('Ctrl Pts',(7.29999794545359,-1.26302231037287,0.690417984675215));
#11336=CARTESIAN_POINT('Ctrl Pts',(7.29999810371711,-1.25834494218995,0.69234933099425));
#11337=CARTESIAN_POINT('Ctrl Pts',(7.29999835129001,-1.25102809722258,0.695370551698293));
#11338=CARTESIAN_POINT('Ctrl Pts',(7.29999895574222,-1.24340909242398,0.6975375590939));
#11339=CARTESIAN_POINT('Ctrl Pts',(7.29999944081525,-1.2356348173965,0.698780605629559));
#11340=CARTESIAN_POINT('Ctrl Pts',(7.29999975409932,-1.23061380764338,0.699583426311495));
#11341=CARTESIAN_POINT('Ctrl Pts',(7.30000000047446,-1.22552743956586,0.699999999832051));
#11342=CARTESIAN_POINT('Ctrl Pts',(7.29999999989087,-1.22041345054982,0.7));
#11343=CARTESIAN_POINT('',(7.3,-1.35236351479115,0.));
#11344=CARTESIAN_POINT('Ctrl Pts',(7.3,-1.35236351479115,0.));
#11345=CARTESIAN_POINT('Ctrl Pts',(7.3,-1.34701814920095,0.100967071798286));
#11346=CARTESIAN_POINT('Ctrl Pts',(7.3,-1.34167252169398,0.201935082699409));
#11347=CARTESIAN_POINT('Ctrl Pts',(7.3,-1.33099009614589,0.403696237111114));
#11348=CARTESIAN_POINT('Ctrl Pts',(7.29999999953133,-1.32565319812959,0.504491283257837));
#11349=CARTESIAN_POINT('Ctrl Pts',(7.29999999953133,-1.3203161347307,0.605285370449834));
#11350=CARTESIAN_POINT('',(7.3,-1.42555555555556,0.));
#11351=CARTESIAN_POINT('Origin',(3.7,-1.44777777777778,0.));
#11352=CARTESIAN_POINT('',(3.7,1.37924639543935,0.));
#11353=CARTESIAN_POINT('',(3.7,-1.44777777777778,0.));
#11354=CARTESIAN_POINT('',(3.7,1.34735368793805,0.605261457205193));
#11355=CARTESIAN_POINT('Ctrl Pts',(3.7,1.34735368793805,0.605261457205193));
#11356=CARTESIAN_POINT('Ctrl Pts',(3.7,1.35266395147774,0.504488703431434));
#11357=CARTESIAN_POINT('Ctrl Pts',(3.7,1.35797406404029,0.40371594170176));
#11358=CARTESIAN_POINT('Ctrl Pts',(3.7,1.36860496587027,0.201962122597264));
#11359=CARTESIAN_POINT('Ctrl Pts',(3.7,1.37392575452088,0.100981065191366));
#11360=CARTESIAN_POINT('Ctrl Pts',(3.7,1.37924639543935,0.));
#11361=CARTESIAN_POINT('',(3.7,1.24747724070879,0.7));
#11362=CARTESIAN_POINT('Ctrl Pts',(3.7,1.24747724070879,0.7));
#11363=CARTESIAN_POINT('Ctrl Pts',(3.7,1.25538532734776,0.7));
#11364=CARTESIAN_POINT('Ctrl Pts',(3.70000034866643,1.26322972530331,0.699006048248363));
#11365=CARTESIAN_POINT('Ctrl Pts',(3.70000065268588,1.27087026624727,0.697119044026295));
#11366=CARTESIAN_POINT('Ctrl Pts',(3.7000008238479,1.27517186762995,0.696056666371322));
#11367=CARTESIAN_POINT('Ctrl Pts',(3.70000097972585,1.27940891103121,0.694710185093394));
#11368=CARTESIAN_POINT('Ctrl Pts',(3.70000107833511,1.28355469746902,0.693090631030141));
#11369=CARTESIAN_POINT('Ctrl Pts',(3.70000125487464,1.29097687270382,0.690191153635441));
#11370=CARTESIAN_POINT('Ctrl Pts',(3.7000012145424,1.29802606517866,0.686451118058958));
#11371=CARTESIAN_POINT('Ctrl Pts',(3.70000098691147,1.3045562506385,0.681952404110064));
#11372=CARTESIAN_POINT('Ctrl Pts',(3.70000086156653,1.30815209635338,0.679475187900035));
#11373=CARTESIAN_POINT('Ctrl Pts',(3.70000068390876,1.31159030769532,0.676767042898431));
#11374=CARTESIAN_POINT('Ctrl Pts',(3.70000052608992,1.31484259178137,0.673836088143417));
#11375=CARTESIAN_POINT('Ctrl Pts',(3.70000037216713,1.31801458722906,0.670977489418868));
#11376=CARTESIAN_POINT('Ctrl Pts',(3.70000023558528,1.32099045552882,0.667924239810466));
#11377=CARTESIAN_POINT('Ctrl Pts',(3.70000023595245,1.32374763345498,0.664687876924229));
#11378=CARTESIAN_POINT('Ctrl Pts',(3.70000023663259,1.32885491153898,0.658692977181302));
#11379=CARTESIAN_POINT('Ctrl Pts',(3.70000065621025,1.33321474659758,0.652071180203097));
#11380=CARTESIAN_POINT('Ctrl Pts',(3.70000080093706,1.33676785491319,0.644988218508662));
#11381=CARTESIAN_POINT('Ctrl Pts',(3.70000081573428,1.33713113341147,0.644264039153811));
#11382=CARTESIAN_POINT('Ctrl Pts',(3.70000082835625,1.33748593861467,0.643535019157411));
#11383=CARTESIAN_POINT('Ctrl Pts',(3.70000083855542,1.33783217873901,0.642801324492746));
#11384=CARTESIAN_POINT('Ctrl Pts',(3.70000093832019,1.34121897990539,0.63562457699476));
#11385=CARTESIAN_POINT('Ctrl Pts',(3.70000072997693,1.34375116782692,0.628085030530103));
#11386=CARTESIAN_POINT('Ctrl Pts',(3.70000042189378,1.34537558692779,0.6203512574804));
#11387=CARTESIAN_POINT('Ctrl Pts',(3.70000022417294,1.3464181026242,0.615387895628485));
#11388=CARTESIAN_POINT('Ctrl Pts',(3.70000000036652,1.34708586836718,0.6103438638189));
#11389=CARTESIAN_POINT('Ctrl Pts',(3.69999999992214,1.34735368792773,0.6052614572053));
#11390=CARTESIAN_POINT('',(3.7,-1.24747724070944,0.7));
#11391=CARTESIAN_POINT('',(3.7,-0.723888888888889,0.7));
#11392=CARTESIAN_POINT('',(3.7,-1.34735368793805,0.605261457205193));
#11393=CARTESIAN_POINT('Ctrl Pts',(3.69999999992215,-1.34735368792773,0.6052614572053));
#11394=CARTESIAN_POINT('Ctrl Pts',(3.70000000061408,-1.34693666923469,0.613175212866596));
#11395=CARTESIAN_POINT('Ctrl Pts',(3.70000049671034,-1.34555248374866,0.620998392122869));
#11396=CARTESIAN_POINT('Ctrl Pts',(3.70000071566022,-1.34328499565267,0.628570462735333));
#11397=CARTESIAN_POINT('Ctrl Pts',(3.70000083807517,-1.34201724238155,0.632804009674372));
#11398=CARTESIAN_POINT('Ctrl Pts',(3.7000008913247,-1.34047237297042,0.63695909738719));
#11399=CARTESIAN_POINT('Ctrl Pts',(3.70000085837557,-1.33865827982058,0.641005656934072));
#11400=CARTESIAN_POINT('Ctrl Pts',(3.7000007994669,-1.33541492172585,0.648240369034365));
#11401=CARTESIAN_POINT('Ctrl Pts',(3.70000042420685,-1.33134915897915,0.655050234746405));
#11402=CARTESIAN_POINT('Ctrl Pts',(3.70000027984635,-1.32652447879733,0.661271863919233));
#11403=CARTESIAN_POINT('Ctrl Pts',(3.70000025294096,-1.32562527203035,0.662431429080655));
#11404=CARTESIAN_POINT('Ctrl Pts',(3.7000002362737,-1.32469957579387,0.663570491348455));
#11405=CARTESIAN_POINT('Ctrl Pts',(3.70000023630138,-1.32374763346102,0.664687876924223));
#11406=CARTESIAN_POINT('Ctrl Pts',(3.70000023635686,-1.32184039796576,0.666926581264246));
#11407=CARTESIAN_POINT('Ctrl Pts',(3.70000030283857,-1.31982784222224,0.669078323867587));
#11408=CARTESIAN_POINT('Ctrl Pts',(3.70000039320883,-1.31771738411303,0.671139279696989));
#11409=CARTESIAN_POINT('Ctrl Pts',(3.70000063660146,-1.3120333248939,0.676690015307994));
#11410=CARTESIAN_POINT('Ctrl Pts',(3.7000010126336,-1.30570602994251,0.681522474044465));
#11411=CARTESIAN_POINT('Ctrl Pts',(3.70000113724274,-1.29889910811053,0.685582059356066));
#11412=CARTESIAN_POINT('Ctrl Pts',(3.70000121634872,-1.29457784995583,0.688159217808216));
#11413=CARTESIAN_POINT('Ctrl Pts',(3.70000121058612,-1.2900623422215,0.690424215862126));
#11414=CARTESIAN_POINT('Ctrl Pts',(3.70000111831253,-1.28538881676413,0.692353818784707));
#11415=CARTESIAN_POINT('Ctrl Pts',(3.70000097388434,-1.27807373536961,0.695374066040565));
#11416=CARTESIAN_POINT('Ctrl Pts',(3.70000061691996,-1.27045659963863,0.697540160564298));
#11417=CARTESIAN_POINT('Ctrl Pts',(3.7000003304055,-1.26268427129293,0.698782316368755));
#11418=CARTESIAN_POINT('Ctrl Pts',(3.70000014548661,-1.25766794365683,0.699584014420239));
#11419=CARTESIAN_POINT('Ctrl Pts',(3.7,-1.25258637988459,0.7));
#11420=CARTESIAN_POINT('Ctrl Pts',(3.7,-1.24747724070879,0.7));
#11421=CARTESIAN_POINT('',(3.7,-1.37924639543935,0.));
#11422=CARTESIAN_POINT('Ctrl Pts',(3.7,-1.37924639543935,0.));
#11423=CARTESIAN_POINT('Ctrl Pts',(3.7,-1.37392574223662,0.100981298335747));
#11424=CARTESIAN_POINT('Ctrl Pts',(3.7,-1.36860494130098,0.201962588887634));
#11425=CARTESIAN_POINT('Ctrl Pts',(3.7,-1.35797403946962,0.403716407992068));
#11426=CARTESIAN_POINT('Ctrl Pts',(3.7,-1.3526639391921,0.504488936575732));
#11427=CARTESIAN_POINT('Ctrl Pts',(3.7,-1.34735368793805,0.605261457205193));
#11428=CARTESIAN_POINT('',(3.7,-1.44777777777778,0.));
#11429=CARTESIAN_POINT('Origin',(1.1,-1.34328341716202,0.));
#11430=CARTESIAN_POINT('',(1.1,1.27885335043294,0.));
#11431=CARTESIAN_POINT('',(1.1,-1.34328341716202,0.));
#11432=CARTESIAN_POINT('Ctrl Pts',(1.1,1.24553911298206,0.605485603995113));
#11433=CARTESIAN_POINT('Ctrl Pts',(1.1,1.25109559382646,0.504544105903265));
#11434=CARTESIAN_POINT('Ctrl Pts',(1.1,1.25665083308595,0.403601248768354));
#11435=CARTESIAN_POINT('Ctrl Pts',(1.1,1.26775551906787,0.201773573764085));
#11436=CARTESIAN_POINT('Ctrl Pts',(1.1,1.2733051088238,0.100886182270816));
#11437=CARTESIAN_POINT('Ctrl Pts',(1.1,1.27885335043294,0.));
#11438=CARTESIAN_POINT('',(1.1,-1.14549341399195,0.7));
#11439=CARTESIAN_POINT('',(1.1,-0.671641708581009,0.7));
#11440=CARTESIAN_POINT('',(1.1,-1.24553911298206,0.605485603995113));
#11441=CARTESIAN_POINT('Ctrl Pts',(1.09999999916631,-1.24553911263843,0.605485603997431));
#11442=CARTESIAN_POINT('Ctrl Pts',(1.10000000220634,-1.24510362317222,0.61339691285734));
#11443=CARTESIAN_POINT('Ctrl Pts',(1.10000177015643,-1.24370036622144,0.621215229994996));
#11444=CARTESIAN_POINT('Ctrl Pts',(1.10000252895322,-1.24141353486351,0.628780213666851));
#11445=CARTESIAN_POINT('Ctrl Pts',(1.10000294802756,-1.24015054543059,0.632958263090869));
#11446=CARTESIAN_POINT('Ctrl Pts',(1.10000312162076,-1.23861706177488,0.637059070655947));
#11447=CARTESIAN_POINT('Ctrl Pts',(1.10000299297862,-1.23682078380192,0.641053713130525));
#11448=CARTESIAN_POINT('Ctrl Pts',(1.10000275999609,-1.23356756237267,0.64828837095969));
#11449=CARTESIAN_POINT('Ctrl Pts',(1.10000138715103,-1.22949085733774,0.655096441442141));
#11450=CARTESIAN_POINT('Ctrl Pts',(1.10000084482056,-1.2246552743941,0.661315040399663));
#11451=CARTESIAN_POINT('Ctrl Pts',(1.10000074196669,-1.22373819809959,0.662494407966206));
#11452=CARTESIAN_POINT('Ctrl Pts',(1.1000006773267,-1.22279369438101,0.663652502541609));
#11453=CARTESIAN_POINT('Ctrl Pts',(1.10000067553493,-1.22182202641035,0.66478809188211));
#11454=CARTESIAN_POINT('Ctrl Pts',(1.10000067210542,-1.219962222636,0.666961646435043));
#11455=CARTESIAN_POINT('Ctrl Pts',(1.10000089707048,-1.21800293160495,0.669052796220007));
#11456=CARTESIAN_POINT('Ctrl Pts',(1.10000120920309,-1.21595100691259,0.671058078730413));
#11457=CARTESIAN_POINT('Ctrl Pts',(1.10000207391986,-1.21026645613745,0.676613414309409));
#11458=CARTESIAN_POINT('Ctrl Pts',(1.1000034579227,-1.20393786500476,0.681450029097565));
#11459=CARTESIAN_POINT('Ctrl Pts',(1.10000394126019,-1.19712964857754,0.685514663758263));
#11460=CARTESIAN_POINT('Ctrl Pts',(1.10000424974863,-1.19278432848208,0.688108902478585));
#11461=CARTESIAN_POINT('Ctrl Pts',(1.10000425197701,-1.18824265871575,0.690387991283085));
#11462=CARTESIAN_POINT('Ctrl Pts',(1.10000394032285,-1.18354156621637,0.692328715646671));
#11463=CARTESIAN_POINT('Ctrl Pts',(1.10000345443802,-1.17621232165581,0.695354404566264));
#11464=CARTESIAN_POINT('Ctrl Pts',(1.10000219938511,-1.16858027633095,0.697525330589554));
#11465=CARTESIAN_POINT('Ctrl Pts',(1.10000118192936,-1.16079305972554,0.698772417158578));
#11466=CARTESIAN_POINT('Ctrl Pts',(1.10000052251962,-1.15574619011492,0.699580649884844));
#11467=CARTESIAN_POINT('Ctrl Pts',(1.1,-1.15063354328712,0.7));
#11468=CARTESIAN_POINT('Ctrl Pts',(1.1,-1.14549341399196,0.7));
#11469=CARTESIAN_POINT('',(1.1,-1.27885335043294,0.));
#11470=CARTESIAN_POINT('Ctrl Pts',(1.1,-1.27885335043294,0.));
#11471=CARTESIAN_POINT('Ctrl Pts',(1.1,-1.27330503870861,0.100887457206881));
#11472=CARTESIAN_POINT('Ctrl Pts',(1.1,-1.26775537880223,0.201776123688554));
#11473=CARTESIAN_POINT('Ctrl Pts',(1.1,-1.25665069275548,0.403603798678134));
#11474=CARTESIAN_POINT('Ctrl Pts',(1.1,-1.25109552364596,0.504545380833391));
#11475=CARTESIAN_POINT('Ctrl Pts',(1.1,-1.24553911298206,0.605485603995113));
#11476=CARTESIAN_POINT('',(1.1,-1.34328341716202,0.));
#11477=CARTESIAN_POINT('Origin',(0.199725906950915,-1.4,-0.0104671912485888));
#11478=CARTESIAN_POINT('',(0.200274469199584,1.12301388185427,1.38777878078145E-17));
#11479=CARTESIAN_POINT('',(0.200274469199585,-0.7,0.));
#11480=CARTESIAN_POINT('',(0.231993417893744,1.09142177001972,0.605233595624295));
#11481=CARTESIAN_POINT('Ctrl Pts',(0.200274469199584,1.12301388185427,-2.97071395261028E-17));
#11482=CARTESIAN_POINT('Ctrl Pts',(0.210847451470635,1.11248294808,0.201744519910852));
#11483=CARTESIAN_POINT('Ctrl Pts',(0.22142043436526,1.101952242875,0.403489051720196));
#11484=CARTESIAN_POINT('Ctrl Pts',(0.231993417893744,1.09142177001972,0.605233595624295));
#11485=CARTESIAN_POINT('',(0.231993417893744,-1.09142177001972,0.605233595624295));
#11486=CARTESIAN_POINT('',(0.231993417893744,-0.7,0.605233595624295));
#11487=CARTESIAN_POINT('',(0.200274469199584,-1.12301388185427,-1.38777878078145E-17));
#11488=CARTESIAN_POINT('Ctrl Pts',(0.231993417893744,-1.09142177001972,
0.605233595624295));
#11489=CARTESIAN_POINT('Ctrl Pts',(0.22142043436526,-1.101952242875,0.403489051720196));
#11490=CARTESIAN_POINT('Ctrl Pts',(0.210847451470635,-1.11248294808,0.201744519910852));
#11491=CARTESIAN_POINT('Ctrl Pts',(0.200274469199584,-1.12301388185427,
-4.90059381963448E-17));
#11492=CARTESIAN_POINT('',(0.200274469199585,-0.7,0.));
#11493=CARTESIAN_POINT('Origin',(5.4,-1.11022302462516E-16,0.));
#11494=CARTESIAN_POINT('Ctrl Pts',(7.29999999999999,-1.35236351479115,1.04083408558608E-17));
#11495=CARTESIAN_POINT('Ctrl Pts',(8.20044803681595,-1.32637404707459,3.18306896032855E-8));
#11496=CARTESIAN_POINT('Ctrl Pts',(9.10060048441536,-1.28803709316692,1.03188250195688E-8));
#11497=CARTESIAN_POINT('Ctrl Pts',(10.0000000000405,-1.24211782537639,-8.23328475353175E-12));
#11498=CARTESIAN_POINT('Ctrl Pts',(10.0000000000405,1.24211782537639,-8.23320567538283E-12));
#11499=CARTESIAN_POINT('Ctrl Pts',(9.1006004808701,1.28803709334794,1.03184817085883E-8));
#11500=CARTESIAN_POINT('Ctrl Pts',(8.20044803144508,1.32637404722969,3.18291413954212E-8));
#11501=CARTESIAN_POINT('Ctrl Pts',(7.3,1.35236351479115,4.75121773919879E-17));
#11502=CARTESIAN_POINT('',(7.1,1.35793097395724,0.));
#11503=CARTESIAN_POINT('',(7.1,1.42555555555556,0.));
#11504=CARTESIAN_POINT('Ctrl Pts',(7.1000000000396,1.35793097389613,-4.88924676637329E-12));
#11505=CARTESIAN_POINT('Ctrl Pts',(6.53177385320612,1.37316067096195,3.71763852401782E-9));
#11506=CARTESIAN_POINT('Ctrl Pts',(5.96344379069665,1.38333257666104,-3.82408184804385E-8));
#11507=CARTESIAN_POINT('Ctrl Pts',(5.39512359652123,1.38725406840392,-3.97623797275691E-8));
#11508=CARTESIAN_POINT('Ctrl Pts',(4.82973248928002,1.39115534902226,-4.12760989429076E-8));
#11509=CARTESIAN_POINT('Ctrl Pts',(4.26470859812609,1.38886839226708,1.63957607983357E-8));
#11510=CARTESIAN_POINT('Ctrl Pts',(3.70000000036239,1.37924639538501,-6.25376529969227E-12));
#11511=CARTESIAN_POINT('',(3.5,1.37552980833516,0.));
#11512=CARTESIAN_POINT('',(3.5,1.44777777777778,0.));
#11513=CARTESIAN_POINT('Ctrl Pts',(3.50000000097466,1.37552980835479,1.06251812903579E-15));
#11514=CARTESIAN_POINT('Ctrl Pts',(2.69943075695685,1.35940904975719,2.35366119539541E-7));
#11515=CARTESIAN_POINT('Ctrl Pts',(1.89948254587541,1.32827224396921,2.51300192353997E-7));
#11516=CARTESIAN_POINT('Ctrl Pts',(1.10000000028363,1.27885335028943,-5.13283415455519E-11));
#11517=CARTESIAN_POINT('',(0.9,1.266106713614,0.));
#11518=CARTESIAN_POINT('',(0.9,1.34328341716202,0.));
#11519=CARTESIAN_POINT('',(0.292382661757373,1.22257596919059,0.));
#11520=CARTESIAN_POINT('Ctrl Pts',(0.9,1.266106713614,1.20346441145891E-16));
#11521=CARTESIAN_POINT('Ctrl Pts',(0.697432754539207,1.25280566772398,-2.10387859372414E-8));
#11522=CARTESIAN_POINT('Ctrl Pts',(0.494894520889663,1.23831317328004,3.6654767345328E-12));
#11523=CARTESIAN_POINT('Ctrl Pts',(0.292382661757371,1.22257596919059,2.98331735103528E-16));
#11524=CARTESIAN_POINT('Ctrl Pts',(0.292382661757373,1.22257596919059,2.94902990916057E-17));
#11525=CARTESIAN_POINT('Ctrl Pts',(0.284469747869226,1.22196105627757,-8.65621238729993E-13));
#11526=CARTESIAN_POINT('Ctrl Pts',(0.276673396002317,1.22038240716686,-1.19564355630166E-6));
#11527=CARTESIAN_POINT('Ctrl Pts',(0.269153172408756,1.21792571627104,-1.29137975931779E-6));
#11528=CARTESIAN_POINT('Ctrl Pts',(0.264330998492885,1.21635041859408,-1.35276844214688E-6));
#11529=CARTESIAN_POINT('Ctrl Pts',(0.259622238853914,1.21441292414196,-1.0165784587106E-6));
#11530=CARTESIAN_POINT('Ctrl Pts',(0.255072584042237,1.21212521597766,-4.21167369976509E-7));
#11531=CARTESIAN_POINT('Ctrl Pts',(0.247984787860257,1.20856125126747,5.06409032217246E-7));
#11532=CARTESIAN_POINT('Ctrl Pts',(0.241364979299678,1.20419126978451,2.25366520907849E-6));
#11533=CARTESIAN_POINT('Ctrl Pts',(0.235375785094684,1.19908071490398,1.28723124315333E-6));
#11534=CARTESIAN_POINT('Ctrl Pts',(0.235058634311792,1.19881009144014,1.23605486142058E-6));
#11535=CARTESIAN_POINT('Ctrl Pts',(0.234743258170683,1.19853738091759,1.17639378419006E-6));
#11536=CARTESIAN_POINT('Ctrl Pts',(0.234429683218046,1.19826258967301,1.10742116603597E-6));
#11537=CARTESIAN_POINT('Ctrl Pts',(0.23095881299434,1.19522100506769,3.4398325561458E-7));
#11538=CARTESIAN_POINT('Ctrl Pts',(0.227708211416394,1.19192479473749,-1.52348441667556E-6));
#11539=CARTESIAN_POINT('Ctrl Pts',(0.224692430858345,1.18840300965977,-3.42436181452249E-6));
#11540=CARTESIAN_POINT('Ctrl Pts',(0.219522873151367,1.18236607466387,-6.68278702580898E-6));
#11541=CARTESIAN_POINT('Ctrl Pts',(0.21509942609515,1.17573654654733,-9.78259773483875E-6));
#11542=CARTESIAN_POINT('Ctrl Pts',(0.211478909386775,1.16867548752938,-1.04320859863301E-5));
#11543=CARTESIAN_POINT('Ctrl Pts',(0.20968494559888,1.16517673715679,-1.075390701291E-5));
#11544=CARTESIAN_POINT('Ctrl Pts',(0.208088728862602,1.16157146972622,-1.05358292927083E-5));
#11545=CARTESIAN_POINT('Ctrl Pts',(0.206701335101202,1.15787708229469,-9.83193564179307E-6));
#11546=CARTESIAN_POINT('Ctrl Pts',(0.203919119965097,1.15046852899383,-8.42037994342582E-6));
#11547=CARTESIAN_POINT('Ctrl Pts',(0.202003457218558,1.1427818296106,-4.88542801801716E-6));
#11548=CARTESIAN_POINT('Ctrl Pts',(0.201024541128784,1.13496408391561,-2.30807221316776E-6));
#11549=CARTESIAN_POINT('Ctrl Pts',(0.200529226009753,1.13100843574523,-1.00397341389412E-6));
#11550=CARTESIAN_POINT('Ctrl Pts',(0.200274469344113,1.12701892049093,-1.14168925800036E-11));
#11551=CARTESIAN_POINT('Ctrl Pts',(0.200274469199584,1.12301388185427,-1.43114686768087E-17));
#11552=CARTESIAN_POINT('',(-1.73234772679968E-18,1.12356026268968,4.53319947845445E-20));
#11553=CARTESIAN_POINT('',(0.,-1.4,0.));
#11554=CARTESIAN_POINT('',(0.276326924564679,1.42224670711126,-2.77555756156289E-17));
#11555=CARTESIAN_POINT('Ctrl Pts',(0.276326924564681,1.42224670711126,-1.50920942409982E-16));
#11556=CARTESIAN_POINT('Ctrl Pts',(0.258529852003869,1.4208638358667,-3.32972379743633E-13));
#11557=CARTESIAN_POINT('Ctrl Pts',(0.240927013527826,1.41785398988725,-1.99727536601662E-6));
#11558=CARTESIAN_POINT('Ctrl Pts',(0.223720619657732,1.41333325652174,-2.71091968639774E-6));
#11559=CARTESIAN_POINT('Ctrl Pts',(0.206313289378911,1.40875972999491,-3.432897951005E-6));
#11560=CARTESIAN_POINT('Ctrl Pts',(0.18931019325249,1.40263932318529,-2.78724979559428E-6));
#11561=CARTESIAN_POINT('Ctrl Pts',(0.172932985028856,1.39504220432096,-6.31841720307455E-7));
#11562=CARTESIAN_POINT('Ctrl Pts',(0.170060146426803,1.39370954151055,-2.53746782677961E-7));
#11563=CARTESIAN_POINT('Ctrl Pts',(0.167206630967902,1.39233132643846,1.61597591574489E-7));
#11564=CARTESIAN_POINT('Ctrl Pts',(0.164373729059928,1.39090779908693,6.02790108062464E-7));
#11565=CARTESIAN_POINT('Ctrl Pts',(0.148213121449433,1.38278712717586,3.11962244863226E-6));
#11566=CARTESIAN_POINT('Ctrl Pts',(0.132864864406694,1.37326763401578,6.8005293729143E-6));
#11567=CARTESIAN_POINT('Ctrl Pts',(0.118540368157823,1.36244192017091,7.47011412280372E-6));
#11568=CARTESIAN_POINT('Ctrl Pts',(0.1130124780146,1.35826422653222,7.72851001154276E-6));
#11569=CARTESIAN_POINT('Ctrl Pts',(0.107637267132642,1.35389150739715,7.50091387420595E-6));
#11570=CARTESIAN_POINT('Ctrl Pts',(0.102427993107927,1.34932731552598,6.39696583889361E-6));
#11571=CARTESIAN_POINT('Ctrl Pts',(0.0920147884934566,1.34020361352282,
4.19020214765608E-6));
#11572=CARTESIAN_POINT('Ctrl Pts',(0.082263696775192,1.33031540618347,-1.43705507633734E-6));
#11573=CARTESIAN_POINT('Ctrl Pts',(0.0732179607829324,1.31975004019149,
-7.24116446069057E-6));
#11574=CARTESIAN_POINT('Ctrl Pts',(0.0614369648181435,1.30598990677343,
-1.48003270644599E-5));
#11575=CARTESIAN_POINT('Ctrl Pts',(0.0509520748529884,1.29120077200215,
-2.24515165560165E-5));
#11576=CARTESIAN_POINT('Ctrl Pts',(0.0418305631051555,1.27560026299671,
-2.64881615939377E-5));
#11577=CARTESIAN_POINT('Ctrl Pts',(0.0329966685655992,1.26049166530727,
-3.03975241584371E-5));
#11578=CARTESIAN_POINT('Ctrl Pts',(0.0254411283904758,1.24462062939249,
-3.09701348507133E-5));
#11579=CARTESIAN_POINT('Ctrl Pts',(0.0192647836588538,1.2281607987719,-2.81763116144976E-5));
#11580=CARTESIAN_POINT('Ctrl Pts',(0.0129258683931997,1.2112677210496,-2.53089508159798E-5));
#11581=CARTESIAN_POINT('Ctrl Pts',(0.00809110271874438,1.19389182855556,
-1.89493195503086E-5));
#11582=CARTESIAN_POINT('Ctrl Pts',(0.00484442764459327,1.17622983835018,
-1.25518552566888E-5));
#11583=CARTESIAN_POINT('Ctrl Pts',(0.00165723550742335,1.1588914367474,
-6.27160009448058E-6));
#11584=CARTESIAN_POINT('Ctrl Pts',(1.90718451428807E-9,1.14127598190669,
-1.51296892603399E-10));
#11585=CARTESIAN_POINT('Ctrl Pts',(2.41777084464267E-17,1.12356026268968,
-3.46944695195361E-18));
#11586=CARTESIAN_POINT('',(10.5166159648474,1.4155315881283,0.));
#11587=CARTESIAN_POINT('Ctrl Pts',(0.276326924564679,1.42224670711126,0.));
#11588=CARTESIAN_POINT('Ctrl Pts',(3.68975660465893,1.68747752195839,0.));
#11589=CARTESIAN_POINT('Ctrl Pts',(7.10318628475318,1.599994843061,0.));
#11590=CARTESIAN_POINT('Ctrl Pts',(10.5166159648474,1.4155315881283,0.));
#11591=CARTESIAN_POINT('',(10.8,1.11638029377732,-5.56631991785941E-17));
#11592=CARTESIAN_POINT('Ctrl Pts',(10.8,1.11638029377732,2.32452945780892E-16));
#11593=CARTESIAN_POINT('Ctrl Pts',(10.7999999994302,1.13421844616111,-9.29296349749781E-12));
#11594=CARTESIAN_POINT('Ctrl Pts',(10.7983603663884,1.15198349698667,-2.38856955364628E-6));
#11595=CARTESIAN_POINT('Ctrl Pts',(10.7951843826221,1.16946861094468,-3.77014304120448E-6));
#11596=CARTESIAN_POINT('Ctrl Pts',(10.7919669771209,1.18718176881198,-5.16973525142236E-6));
#11597=CARTESIAN_POINT('Ctrl Pts',(10.7871724978816,1.20460918321158,-5.4755482503851E-6));
#11598=CARTESIAN_POINT('Ctrl Pts',(10.7808573412527,1.22152732075962,-4.27334038376583E-6));
#11599=CARTESIAN_POINT('Ctrl Pts',(10.7797421066656,1.22451500471617,-4.06103467663179E-6));
#11600=CARTESIAN_POINT('Ctrl Pts',(10.7785793293545,1.22748675045939,-3.81081650224554E-6));
#11601=CARTESIAN_POINT('Ctrl Pts',(10.7773691713543,1.23044124224994,-3.53261416912234E-6));
#11602=CARTESIAN_POINT('Ctrl Pts',(10.7705159051166,1.24717287467681,-1.95712183132163E-6));
#11603=CARTESIAN_POINT('Ctrl Pts',(10.7622076549587,1.26320448426569,8.50150473021234E-7));
#11604=CARTESIAN_POINT('Ctrl Pts',(10.7525236566209,1.27832128496499,1.09915986206012E-6));
#11605=CARTESIAN_POINT('Ctrl Pts',(10.7482509716548,1.28499098118248,1.20902550183604E-6));
#11606=CARTESIAN_POINT('Ctrl Pts',(10.7437098328292,1.29148238441373,7.76315258636623E-7));
#11607=CARTESIAN_POINT('Ctrl Pts',(10.7389041877712,1.29777551763099,-7.54184826032082E-7));
#11608=CARTESIAN_POINT('Ctrl Pts',(10.7310976851069,1.30799836193882,-3.24039694621926E-6));
#11609=CARTESIAN_POINT('Ctrl Pts',(10.7225935645301,1.31769858917671,-8.57388820182801E-6));
#11610=CARTESIAN_POINT('Ctrl Pts',(10.7134588931078,1.3268364513864,-1.41086939541967E-5));
#11611=CARTESIAN_POINT('Ctrl Pts',(10.7004433550849,1.33985653580309,-2.19949628070403E-5));
#11612=CARTESIAN_POINT('Ctrl Pts',(10.6862650266646,1.35162127070648,-3.0022236679635E-5));
#11613=CARTESIAN_POINT('Ctrl Pts',(10.6711476119081,1.36204513612776,-3.40981369893719E-5));
#11614=CARTESIAN_POINT('Ctrl Pts',(10.6560301971515,1.37246900154903,-3.81740372991087E-5));
#11615=CARTESIAN_POINT('Ctrl Pts',(10.6399721826852,1.38155285075117,-3.83332859284948E-5));
#11616=CARTESIAN_POINT('Ctrl Pts',(10.6231652498763,1.38916602817047,-3.45204725343976E-5));
#11617=CARTESIAN_POINT('Ctrl Pts',(10.6063487480974,1.39678354012646,-3.07054883279539E-5));
#11618=CARTESIAN_POINT('Ctrl Pts',(10.5889271210941,1.40286310406803,-2.29928881382306E-5));
#11619=CARTESIAN_POINT('Ctrl Pts',(10.5711041279812,1.40730078588308,-1.53078138731408E-5));
#11620=CARTESIAN_POINT('Ctrl Pts',(10.5532811348684,1.41173846769814,-7.6227396080509E-6));
#11621=CARTESIAN_POINT('Ctrl Pts',(10.5350552605908,1.41453511891929,-9.16729947674095E-11));
#11622=CARTESIAN_POINT('Ctrl Pts',(10.5166159648474,1.4155315881283,2.48932818802672E-16));
#11623=CARTESIAN_POINT('',(10.8,-1.11638029377732,-1.39157997946485E-17));
#11624=CARTESIAN_POINT('',(10.8,1.4,0.));
#11625=CARTESIAN_POINT('',(10.5166159648474,-1.4155315881283,2.77555756156289E-17));
#11626=CARTESIAN_POINT('Ctrl Pts',(10.5166159648474,-1.4155315881283,-1.94289029309402E-16));
#11627=CARTESIAN_POINT('Ctrl Pts',(10.5344251606169,-1.41456917089032,1.72780596414851E-12));
#11628=CARTESIAN_POINT('Ctrl Pts',(10.5520727686739,-1.41197333457428,-2.53403886306205E-6));
#11629=CARTESIAN_POINT('Ctrl Pts',(10.5693578805681,-1.40785843881911,-4.04156906196095E-6));
#11630=CARTESIAN_POINT('Ctrl Pts',(10.5868701251756,-1.40368947182374,-5.56890876087065E-6));
#11631=CARTESIAN_POINT('Ctrl Pts',(10.604011804524,-1.39796079212135,-5.98742339745246E-6));
#11632=CARTESIAN_POINT('Ctrl Pts',(10.6205627760847,-1.39074087128671,-4.81856832951796E-6));
#11633=CARTESIAN_POINT('Ctrl Pts',(10.6234754753687,-1.38947028374636,-4.61286902618664E-6));
#11634=CARTESIAN_POINT('Ctrl Pts',(10.6263698187278,-1.38815339768352,-4.36721670635639E-6));
#11635=CARTESIAN_POINT('Ctrl Pts',(10.629244514885,-1.38679044403738,-4.09122931699412E-6));
#11636=CARTESIAN_POINT('Ctrl Pts',(10.6455827855986,-1.37904412775797,-2.5226612199239E-6));
#11637=CARTESIAN_POINT('Ctrl Pts',(10.6611432679573,-1.36988219838444,3.58605122725343E-7));
#11638=CARTESIAN_POINT('Ctrl Pts',(10.6757157985124,-1.35939560704671,7.40589063327193E-7));
#11639=CARTESIAN_POINT('Ctrl Pts',(10.6821516119741,-1.35476430808026,9.09288478831296E-7));
#11640=CARTESIAN_POINT('Ctrl Pts',(10.6883944859408,-1.34987400891586,5.44816430868337E-7));
#11641=CARTESIAN_POINT('Ctrl Pts',(10.6944246343503,-1.34472976213865,-9.14752338109426E-7));
#11642=CARTESIAN_POINT('Ctrl Pts',(10.7041966733629,-1.33639335368171,-3.28002794718031E-6));
#11643=CARTESIAN_POINT('Ctrl Pts',(10.7134106653983,-1.3273903805878,-8.47259327327479E-6));
#11644=CARTESIAN_POINT('Ctrl Pts',(10.7220307555455,-1.31778973409553,-1.38734771921913E-5));
#11645=CARTESIAN_POINT('Ctrl Pts',(10.7343338492722,-1.3040871333553,-2.15819326638919E-5));
#11646=CARTESIAN_POINT('Ctrl Pts',(10.7453199276401,-1.28929041974124,-2.94555326738194E-5));
#11647=CARTESIAN_POINT('Ctrl Pts',(10.7549158277293,-1.27362793268665,-3.3443536645081E-5));
#11648=CARTESIAN_POINT('Ctrl Pts',(10.7645117278185,-1.25796544563206,-3.74315406163426E-5));
#11649=CARTESIAN_POINT('Ctrl Pts',(10.7727182208071,-1.24143562566754,-3.75750290962259E-5));
#11650=CARTESIAN_POINT('Ctrl Pts',(10.7794153247677,-1.22423716044977,-3.38265125308188E-5));
#11651=CARTESIAN_POINT('Ctrl Pts',(10.7861166764432,-1.20702778690835,-3.00756184258222E-5));
#11652=CARTESIAN_POINT('Ctrl Pts',(10.7912490477072,-1.18929683429644,-2.25107044755726E-5));
#11653=CARTESIAN_POINT('Ctrl Pts',(10.7947196858669,-1.17125359626911,-1.49815203503087E-5));
#11654=CARTESIAN_POINT('Ctrl Pts',(10.7981903240266,-1.15321035824179,-7.45233622504479E-6));
#11655=CARTESIAN_POINT('Ctrl Pts',(10.7999999985278,-1.13485327409571,-1.17780195603766E-10));
#11656=CARTESIAN_POINT('Ctrl Pts',(10.8,-1.11638029377732,-1.38777878078145E-17));
#11657=CARTESIAN_POINT('',(0.276326924564679,-1.42224670711126,-5.55111512312578E-17));
#11658=CARTESIAN_POINT('Ctrl Pts',(10.5166159648474,-1.4155315881283,0.));
#11659=CARTESIAN_POINT('Ctrl Pts',(7.10318628475318,-1.599994843061,0.));
#11660=CARTESIAN_POINT('Ctrl Pts',(3.68975660465893,-1.68747752195839,0.));
#11661=CARTESIAN_POINT('Ctrl Pts',(0.276326924564679,-1.42224670711126,
0.));
#11662=CARTESIAN_POINT('',(-7.25311916552711E-19,-1.12356026268968,1.39157997946485E-17));
#11663=CARTESIAN_POINT('Ctrl Pts',(1.80411241501588E-16,-1.12356026268968,
-1.53523027623947E-16));
#11664=CARTESIAN_POINT('Ctrl Pts',(7.41078168374529E-10,-1.14141522098415,
-1.3067981184062E-11));
#11665=CARTESIAN_POINT('Ctrl Pts',(0.00163694718329378,-1.15920272117896,
-1.78823819589733E-6));
#11666=CARTESIAN_POINT('Ctrl Pts',(0.00481087395297265,-1.17671209893291,
-2.3181425555783E-6));
#11667=CARTESIAN_POINT('Ctrl Pts',(0.00802138847203439,-1.19442331774104,
-2.85415543927884E-6));
#11668=CARTESIAN_POINT('Ctrl Pts',(0.0128049030182357,-1.21185152247087,
-2.04128886843626E-6));
#11669=CARTESIAN_POINT('Ctrl Pts',(0.0191087770915565,-1.22877027194193,
1.71240493184593E-7));
#11670=CARTESIAN_POINT('Ctrl Pts',(0.0202201941454154,-1.23175316571065,
5.613248819379E-7));
#11671=CARTESIAN_POINT('Ctrl Pts',(0.0213789882593307,-1.23472016785247,
9.85829603970989E-7));
#11672=CARTESIAN_POINT('Ctrl Pts',(0.0225850188675993,-1.23766995297306,
1.43287414332239E-6));
#11673=CARTESIAN_POINT('Ctrl Pts',(0.0294291562303479,-1.25440977235863,
3.96981990042924E-6));
#11674=CARTESIAN_POINT('Ctrl Pts',(0.0377300686697735,-1.27044838970616,
7.55798501181421E-6));
#11675=CARTESIAN_POINT('Ctrl Pts',(0.0474121614036163,-1.28556782977674,
8.05058320302158E-6));
#11676=CARTESIAN_POINT('Ctrl Pts',(0.0511425121829324,-1.29139310088294,
8.24037316857697E-6));
#11677=CARTESIAN_POINT('Ctrl Pts',(0.0550784035723718,-1.29708174651376,
7.93435480917585E-6));
#11678=CARTESIAN_POINT('Ctrl Pts',(0.0592173503759339,-1.30262033374061,
6.74858081742264E-6));
#11679=CARTESIAN_POINT('Ctrl Pts',(0.0675201807396794,-1.31373087764993,
4.36988865960166E-6));
#11680=CARTESIAN_POINT('Ctrl Pts',(0.0766394565597649,-1.32423847988766,
-1.46587651676554E-6));
#11681=CARTESIAN_POINT('Ctrl Pts',(0.0864911062490747,-1.33409287340636,
-7.46705500292641E-6));
#11682=CARTESIAN_POINT('Ctrl Pts',(0.0992988409846585,-1.34690417528452,
-1.52689465211603E-5));
#11683=CARTESIAN_POINT('Ctrl Pts',(0.113232871116931,-1.35850278376499,
-2.31308069859054E-5));
#11684=CARTESIAN_POINT('Ctrl Pts',(0.128081622025101,-1.36880445085772,
-2.72849174168177E-5));
#11685=CARTESIAN_POINT('Ctrl Pts',(0.142447925282442,-1.37877140864598,
-3.13040575171566E-5));
#11686=CARTESIAN_POINT('Ctrl Pts',(0.157671864768995,-1.38752483454192,
-3.1899138628041E-5));
#11687=CARTESIAN_POINT('Ctrl Pts',(0.173588691395025,-1.39495074934422,
-2.90326641197332E-5));
#11688=CARTESIAN_POINT('Ctrl Pts',(0.189936400238013,-1.40257769006131,
-2.60885916756054E-5));
#11689=CARTESIAN_POINT('Ctrl Pts',(0.206881864105471,-1.40874232120582,
-1.95409011442111E-5));
#11690=CARTESIAN_POINT('Ctrl Pts',(0.22423558959196,-1.41334558507228,-1.29462590315495E-5));
#11691=CARTESIAN_POINT('Ctrl Pts',(0.241260467995769,-1.4178616186841,-6.47658310103417E-6));
#11692=CARTESIAN_POINT('Ctrl Pts',(0.258679581942429,-1.42087546890512,
-1.12101563992788E-10));
#11693=CARTESIAN_POINT('Ctrl Pts',(0.27632692456468,-1.42224670711126,1.05818132034585E-16));
#11694=CARTESIAN_POINT('',(0.,-1.4,0.));
#11695=CARTESIAN_POINT('',(0.292382661757373,-1.22257596919059,0.));
#11696=CARTESIAN_POINT('Ctrl Pts',(0.200274469199584,-1.12301388185427,
-2.68882138776405E-17));
#11697=CARTESIAN_POINT('Ctrl Pts',(0.200274469314753,-1.13095194822878,
-2.85686379674833E-12));
#11698=CARTESIAN_POINT('Ctrl Pts',(0.201244085522878,-1.13884856843413,
-1.08105759021766E-6));
#11699=CARTESIAN_POINT('Ctrl Pts',(0.203110344361254,-1.14653799330522,
-1.10782444979703E-6));
#11700=CARTESIAN_POINT('Ctrl Pts',(0.204308287281872,-1.15147379958167,
-1.12500597321754E-6));
#11701=CARTESIAN_POINT('Ctrl Pts',(0.205876831658669,-1.15632444796435,
-7.573778542164E-7));
#11702=CARTESIAN_POINT('Ctrl Pts',(0.207807574899602,-1.16104329283393,
-1.57887042599725E-7));
#11703=CARTESIAN_POINT('Ctrl Pts',(0.21096922807971,-1.1687705506961,8.23798139982571E-7));
#11704=CARTESIAN_POINT('Ctrl Pts',(0.215060220496011,-1.17605061753432,
2.67511715935828E-6));
#11705=CARTESIAN_POINT('Ctrl Pts',(0.220020901709485,-1.18268777995331,
1.20301732358232E-6));
#11706=CARTESIAN_POINT('Ctrl Pts',(0.222788929945646,-1.18639127392786,
3.81595076007225E-7));
#11707=CARTESIAN_POINT('Ctrl Pts',(0.225828882930032,-1.18989419630164,
-1.55522758636672E-6));
#11708=CARTESIAN_POINT('Ctrl Pts',(0.229112809647272,-1.19317965616817,
-3.52099818518546E-6));
#11709=CARTESIAN_POINT('Ctrl Pts',(0.234731790749985,-1.1988012605745,-6.88454091865859E-6));
#11710=CARTESIAN_POINT('Ctrl Pts',(0.240999377733319,-1.20372479786492,
-1.00686973618824E-5));
#11711=CARTESIAN_POINT('Ctrl Pts',(0.247759525934523,-1.2078808899968,-1.07387199666626E-5));
#11712=CARTESIAN_POINT('Ctrl Pts',(0.251104201987095,-1.20993717358883,
-1.10702228411842E-5));
#11713=CARTESIAN_POINT('Ctrl Pts',(0.254570062984725,-1.21180502729412,
-1.08478245319173E-5));
#11714=CARTESIAN_POINT('Ctrl Pts',(0.258140701417296,-1.21347208138814,
-1.01264154182862E-5));
#11715=CARTESIAN_POINT('Ctrl Pts',(0.265309933881728,-1.21681924144269,
-8.67794906268977E-6));
#11716=CARTESIAN_POINT('Ctrl Pts',(0.27282354441991,-1.21932394229889,-5.03816435877804E-6));
#11717=CARTESIAN_POINT('Ctrl Pts',(0.280540402387729,-1.22090470300999,
-2.38011023443526E-6));
#11718=CARTESIAN_POINT('Ctrl Pts',(0.284441227387562,-1.22170376798259,
-1.03647996128718E-6));
#11719=CARTESIAN_POINT('Ctrl Pts',(0.288394358015454,-1.22226603782358,
-8.41267709508591E-12));
#11720=CARTESIAN_POINT('Ctrl Pts',(0.292382661757373,-1.22257596919059,
3.10081821330854E-17));
#11721=CARTESIAN_POINT('',(0.9,-1.266106713614,0.));
#11722=CARTESIAN_POINT('Ctrl Pts',(0.29238266175737,-1.22257596919059,3.4274341177698E-16));
#11723=CARTESIAN_POINT('Ctrl Pts',(0.494894519961671,-1.23831317320793,
3.6654050078524E-12));
#11724=CARTESIAN_POINT('Ctrl Pts',(0.697432753591781,-1.25280566766171,
-2.10377631034678E-8));
#11725=CARTESIAN_POINT('Ctrl Pts',(0.900000000000002,-1.266106713614,4.80511808774455E-17));
#11726=CARTESIAN_POINT('',(0.9,1.34328341716202,0.));
#11727=CARTESIAN_POINT('',(3.5,-1.37552980833516,0.));
#11728=CARTESIAN_POINT('Ctrl Pts',(1.10000000028363,-1.27885335028943,-5.13283219638443E-11));
#11729=CARTESIAN_POINT('Ctrl Pts',(1.8994825293422,-1.32827224294784,2.51289069808066E-7));
#11730=CARTESIAN_POINT('Ctrl Pts',(2.69943073922525,-1.35940904940056,2.35357980118634E-7));
#11731=CARTESIAN_POINT('Ctrl Pts',(3.50000000097418,-1.37552980835478,8.59034485311056E-16));
#11732=CARTESIAN_POINT('',(3.5,1.44777777777778,0.));
#11733=CARTESIAN_POINT('',(7.1,-1.35793097395724,0.));
#11734=CARTESIAN_POINT('Ctrl Pts',(3.700000000362,-1.379246395385,-6.25385501848083E-12));
#11735=CARTESIAN_POINT('Ctrl Pts',(4.26467016042339,-1.38886773733237,1.63880713394601E-8));
#11736=CARTESIAN_POINT('Ctrl Pts',(4.82965558050887,-1.39115503781354,-4.12727732537403E-8));
#11737=CARTESIAN_POINT('Ctrl Pts',(5.39500817395676,-1.38725486475042,-3.97626883737645E-8));
#11738=CARTESIAN_POINT('Ctrl Pts',(5.96336684492344,-1.38333395379258,-3.82445741104923E-8));
#11739=CARTESIAN_POINT('Ctrl Pts',(6.53173538886785,-1.37316170188981,3.71969681223073E-9));
#11740=CARTESIAN_POINT('Ctrl Pts',(7.1000000000396,-1.35793097389613,-4.88946831112289E-12));
#11741=CARTESIAN_POINT('',(7.1,1.42555555555556,0.));
#11742=CARTESIAN_POINT('',(10.2,-1.23178301601145,0.));
#11743=CARTESIAN_POINT('',(10.5052647440597,-1.21555035534119,0.));
#11744=CARTESIAN_POINT('Ctrl Pts',(10.2,-1.23178301601145,-4.56855690431079E-17));
#11745=CARTESIAN_POINT('Ctrl Pts',(10.3017652114452,-1.22646242153193,-6.28718440835499E-11));
#11746=CARTESIAN_POINT('Ctrl Pts',(10.4035203469111,-1.22104923788321,1.43982679105611E-13));
#11747=CARTESIAN_POINT('Ctrl Pts',(10.5052647440597,-1.21555035534119,6.44897004721534E-17));
#11748=CARTESIAN_POINT('',(10.5997255308004,-1.11583328740478,1.38777878078145E-17));
#11749=CARTESIAN_POINT('Ctrl Pts',(10.5052647440597,-1.21555035534119,-1.86482773667507E-17));
#11750=CARTESIAN_POINT('Ctrl Pts',(10.5131888530666,-1.21512208850275,-5.60416335832109E-13));
#11751=CARTESIAN_POINT('Ctrl Pts',(10.5210180054001,-1.21372544600509,-1.35972994235015E-6));
#11752=CARTESIAN_POINT('Ctrl Pts',(10.5285917824072,-1.2114444991589,-1.66070161277884E-6));
#11753=CARTESIAN_POINT('Ctrl Pts',(10.5334522234388,-1.20998071066451,-1.8538489757029E-6));
#11754=CARTESIAN_POINT('Ctrl Pts',(10.538207639053,-1.20815156029678,-1.66445033219183E-6));
#11755=CARTESIAN_POINT('Ctrl Pts',(10.542812250732,-1.20596855068549,-1.19054254011085E-6));
#11756=CARTESIAN_POINT('Ctrl Pts',(10.5499808226381,-1.20256998801374,-4.52751316616249E-7));
#11757=CARTESIAN_POINT('Ctrl Pts',(10.5567010840309,-1.19835579238971,1.16775294480959E-6));
#11758=CARTESIAN_POINT('Ctrl Pts',(10.5628099082467,-1.1933896765605,3.12218506849373E-7));
#11759=CARTESIAN_POINT('Ctrl Pts',(10.563392699667,-1.1929159013142,2.30599178383296E-7));
#11760=CARTESIAN_POINT('Ctrl Pts',(10.563969906567,-1.19243524850296,1.23643260424227E-7));
#11761=CARTESIAN_POINT('Ctrl Pts',(10.5645413730323,-1.19194775268147,-1.33988689923433E-8));
#11762=CARTESIAN_POINT('Ctrl Pts',(10.5677990734116,-1.18916873515523,-7.94620907596477E-7));
#11763=CARTESIAN_POINT('Ctrl Pts',(10.5708705204042,-1.18616755700159,-2.52696578471864E-6));
#11764=CARTESIAN_POINT('Ctrl Pts',(10.5737438185805,-1.18296717200411,-4.3349897000341E-6));
#11765=CARTESIAN_POINT('Ctrl Pts',(10.579054042416,-1.17705244973962,-7.67644996655303E-6));
#11766=CARTESIAN_POINT('Ctrl Pts',(10.5836289246435,-1.17052745137283,-1.0999028846932E-5));
#11767=CARTESIAN_POINT('Ctrl Pts',(10.5874112735695,-1.16355342251842,-1.18035167459916E-5));
#11768=CARTESIAN_POINT('Ctrl Pts',(10.5894705469099,-1.15975646143,-1.22415145393192E-5));
#11769=CARTESIAN_POINT('Ctrl Pts',(10.5912942421259,-1.15582570378367,-1.20038889321768E-5));
#11770=CARTESIAN_POINT('Ctrl Pts',(10.5928674986933,-1.15178403025788,-1.11465830745351E-5));
#11771=CARTESIAN_POINT('Ctrl Pts',(10.5957384082276,-1.14440870489779,-9.58215448007377E-6));
#11772=CARTESIAN_POINT('Ctrl Pts',(10.5977463817932,-1.13674651935037,-5.80208140981121E-6));
#11773=CARTESIAN_POINT('Ctrl Pts',(10.5988207707371,-1.12894377506163,-2.8960211281105E-6));
#11774=CARTESIAN_POINT('Ctrl Pts',(10.5994175893465,-1.12460938291963,-1.28171667533415E-6));
#11775=CARTESIAN_POINT('Ctrl Pts',(10.5997255306822,-1.12023121224821,-9.4020583932734E-12));
#11776=CARTESIAN_POINT('Ctrl Pts',(10.5997255308004,-1.11583328740478,-9.97465998686664E-18));
#11777=CARTESIAN_POINT('',(10.5997255308004,1.11583328740478,0.));
#11778=CARTESIAN_POINT('',(10.5997255308004,0.7,0.));
#11779=CARTESIAN_POINT('',(10.5052647440597,1.21555035534119,0.));
#11780=CARTESIAN_POINT('Ctrl Pts',(10.5997255308004,1.11583328740478,8.8037216405823E-17));
#11781=CARTESIAN_POINT('Ctrl Pts',(10.5997255307124,1.12376989384288,-2.22024716398596E-12));
#11782=CARTESIAN_POINT('Ctrl Pts',(10.5987536115518,1.13166401228391,-1.27532141444775E-6));
#11783=CARTESIAN_POINT('Ctrl Pts',(10.5968849989732,1.13935090273995,-1.5236651967046E-6));
#11784=CARTESIAN_POINT('Ctrl Pts',(10.5956849616024,1.14428748291596,-1.68315348385219E-6));
#11785=CARTESIAN_POINT('Ctrl Pts',(10.5941139374364,1.14913880701507,-1.46899737395989E-6));
#11786=CARTESIAN_POINT('Ctrl Pts',(10.5921809408638,1.1538584293407,-9.90118991603547E-7));
#11787=CARTESIAN_POINT('Ctrl Pts',(10.5891742477341,1.16119959911942,-2.45244239835432E-7));
#11788=CARTESIAN_POINT('Ctrl Pts',(10.5853292249979,1.16813727090899,1.33309554558619E-6));
#11789=CARTESIAN_POINT('Ctrl Pts',(10.5807005079991,1.17450509276749,4.08358240744415E-7));
#11790=CARTESIAN_POINT('Ctrl Pts',(10.5802604812716,1.17511044665166,3.20448539159982E-7));
#11791=CARTESIAN_POINT('Ctrl Pts',(10.5798133373602,1.17571063303672,2.07176952714776E-7));
#11792=CARTESIAN_POINT('Ctrl Pts',(10.5793591019426,1.17630549598644,6.38823567561716E-8));
#11793=CARTESIAN_POINT('Ctrl Pts',(10.5767566952267,1.17971358631841,-7.57081408668461E-7));
#11794=CARTESIAN_POINT('Ctrl Pts',(10.5739217504488,1.18294722379721,-2.53660858190298E-6));
#11795=CARTESIAN_POINT('Ctrl Pts',(10.570876618072,1.18599321478588,-4.38998728286835E-6));
#11796=CARTESIAN_POINT('Ctrl Pts',(10.5652565693637,1.19161484813492,-7.81055403847458E-6));
#11797=CARTESIAN_POINT('Ctrl Pts',(10.5589874561388,1.19653507038546,-1.11999964534866E-5));
#11798=CARTESIAN_POINT('Ctrl Pts',(10.5522271124844,1.20068789486255,-1.20263298844839E-5));
#11799=CARTESIAN_POINT('Ctrl Pts',(10.5485500617744,1.20294667739977,-1.24757848359648E-5));
#11800=CARTESIAN_POINT('Ctrl Pts',(10.5447269560479,1.20497781184918,-1.22374322375965E-5));
#11801=CARTESIAN_POINT('Ctrl Pts',(10.5407797717187,1.20676523914267,-1.13674773191707E-5));
#11802=CARTESIAN_POINT('Ctrl Pts',(10.5335711832013,1.210029547771,-9.77871264224002E-6));
#11803=CARTESIAN_POINT('Ctrl Pts',(10.5260296312848,1.21244761587922,-5.9245235663186E-6));
#11804=CARTESIAN_POINT('Ctrl Pts',(10.5182973307397,1.21394093281975,-2.95733858081469E-6));
#11805=CARTESIAN_POINT('Ctrl Pts',(10.514004731837,1.21476995008607,-1.31010113336685E-6));
#11806=CARTESIAN_POINT('Ctrl Pts',(10.5096528988527,1.21531319279956,-7.28166367327128E-12));
#11807=CARTESIAN_POINT('Ctrl Pts',(10.5052647440597,1.21555035534119,-3.31765864780564E-17));
#11808=CARTESIAN_POINT('',(10.2,1.23178301601145,0.));
#11809=CARTESIAN_POINT('Ctrl Pts',(10.5052647440597,1.21555035534119,1.20285454773689E-16));
#11810=CARTESIAN_POINT('Ctrl Pts',(10.4035203468995,1.22104923788384,1.44021921739714E-13));
#11811=CARTESIAN_POINT('Ctrl Pts',(10.3017652114309,1.22646242153268,-6.28696045710378E-11));
#11812=CARTESIAN_POINT('Ctrl Pts',(10.2,1.23178301601145,1.23125603768043E-16));
#11813=CARTESIAN_POINT('',(10.2,-1.30754691548544,0.));
#11814=CARTESIAN_POINT('Origin',(8.8,0.,0.));
#11815=CARTESIAN_POINT('',(8.4,-4.89858719658942E-17,0.));
#11816=CARTESIAN_POINT('Origin',(2.,0.,0.));
#11817=CARTESIAN_POINT('',(1.6,-4.89858719658941E-17,0.7));
#11818=CARTESIAN_POINT('Origin',(2.,0.,0.7));
#11819=CARTESIAN_POINT('',(1.6,-4.89858719658941E-17,0.));
#11820=CARTESIAN_POINT('Origin',(10.2,-1.30754691548544,0.));
#11821=CARTESIAN_POINT('',(10.1999999975107,-1.19856231453552,0.605472757505173));
#11822=CARTESIAN_POINT('Ctrl Pts',(10.2,-1.23178301601145,0.));
#11823=CARTESIAN_POINT('Ctrl Pts',(10.2,-1.22625045235593,0.100869147801815));
#11824=CARTESIAN_POINT('Ctrl Pts',(10.2,-1.22071692450357,0.201739022585575));
#11825=CARTESIAN_POINT('Ctrl Pts',(10.2,-1.2096433936729,0.403562754186249));
#11826=CARTESIAN_POINT('Ctrl Pts',(10.1999999975107,-1.20410330368611,0.50451817268257));
#11827=CARTESIAN_POINT('Ctrl Pts',(10.1999999975107,-1.19856231453552,0.605472757505173));
#11828=CARTESIAN_POINT('',(10.1999999975107,1.19856231453552,0.605472757505173));
#11829=CARTESIAN_POINT('Ctrl Pts',(10.1999999975107,1.19856231453552,0.605472757505173));
#11830=CARTESIAN_POINT('Ctrl Pts',(10.1999999975107,1.20410418062036,0.504502195294633));
#11831=CARTESIAN_POINT('Ctrl Pts',(10.2,1.20964514726505,0.403530798997214));
#11832=CARTESIAN_POINT('Ctrl Pts',(10.2,1.22071867750565,0.201707067365009));
#11833=CARTESIAN_POINT('Ctrl Pts',(10.2,1.22625132869937,0.100853170395858));
#11834=CARTESIAN_POINT('Ctrl Pts',(10.2,1.23178301601145,0.));
#11835=CARTESIAN_POINT('',(10.1999999980542,1.09857320530976,0.7));
#11836=CARTESIAN_POINT('Ctrl Pts',(10.1999999999973,1.09857320510493,0.7));
#11837=CARTESIAN_POINT('Ctrl Pts',(10.2000000008642,1.10649088744708,0.699999999248278));
#11838=CARTESIAN_POINT('Ctrl Pts',(10.1999989363772,1.11434529358656,0.699006164779054));
#11839=CARTESIAN_POINT('Ctrl Pts',(10.1999980093114,1.12199598895487,0.697118997523365));
#11840=CARTESIAN_POINT('Ctrl Pts',(10.1999974900707,1.12628106973794,0.696062013320951));
#11841=CARTESIAN_POINT('Ctrl Pts',(10.1999970168623,1.13050229860485,0.694723760583242));
#11842=CARTESIAN_POINT('Ctrl Pts',(10.199996713894,1.13463332887353,0.693115046692397));
#11843=CARTESIAN_POINT('Ctrl Pts',(10.1999961690675,1.14206214329588,0.690222103243312));
#11844=CARTESIAN_POINT('Ctrl Pts',(10.1999962772589,1.14911941279843,0.686488866209959));
#11845=CARTESIAN_POINT('Ctrl Pts',(10.1999969599022,1.15565885618684,0.681996408643444));
#11846=CARTESIAN_POINT('Ctrl Pts',(10.1999973343062,1.15924549304116,0.679532465931891));
#11847=CARTESIAN_POINT('Ctrl Pts',(10.1999978674396,1.16267609380848,0.676839263748528));
#11848=CARTESIAN_POINT('Ctrl Pts',(10.1999983417863,1.16592263776853,0.673924718551186));
#11849=CARTESIAN_POINT('Ctrl Pts',(10.199998806773,1.16910511991263,0.671067684066867));
#11850=CARTESIAN_POINT('Ctrl Pts',(10.1999992207276,1.17209141256199,0.668015240668471));
#11851=CARTESIAN_POINT('Ctrl Pts',(10.1999992206607,1.17485880184773,0.664778864469812));
#11852=CARTESIAN_POINT('Ctrl Pts',(10.1999992205369,1.17997899231675,0.658790960038769));
#11853=CARTESIAN_POINT('Ctrl Pts',(10.1999979581638,1.18435276586188,0.652174799271591));
#11854=CARTESIAN_POINT('Ctrl Pts',(10.1999975326045,1.18791964688485,0.645095405674036));
#11855=CARTESIAN_POINT('Ctrl Pts',(10.1999974898604,1.18827791229431,0.644384335742179));
#11856=CARTESIAN_POINT('Ctrl Pts',(10.1999974535047,1.18862799840101,0.643668573506599));
#11857=CARTESIAN_POINT('Ctrl Pts',(10.1999974242393,1.18896981696374,0.64294827577739));
#11858=CARTESIAN_POINT('Ctrl Pts',(10.1999971329942,1.1923715530028,0.635779961907205));
#11859=CARTESIAN_POINT('Ctrl Pts',(10.1999977790614,1.19491900203126,0.628247233077589));
#11860=CARTESIAN_POINT('Ctrl Pts',(10.1999987199397,1.19655829940385,0.620518158911201));
#11861=CARTESIAN_POINT('Ctrl Pts',(10.1999993222661,1.19760773597399,0.615570201805241));
#11862=CARTESIAN_POINT('Ctrl Pts',(10.2,1.19828413277105,0.610541112135461));
#11863=CARTESIAN_POINT('Ctrl Pts',(10.2,1.19856231427281,0.60547275750556));
#11864=CARTESIAN_POINT('',(10.2,-1.09857320510402,0.7));
#11865=CARTESIAN_POINT('',(10.2,-0.653773457742722,0.7));
#11866=CARTESIAN_POINT('Ctrl Pts',(10.2,-1.19856231427281,0.60547275750556));
#11867=CARTESIAN_POINT('Ctrl Pts',(10.2,-1.19812809376428,0.613384079828744));
#11868=CARTESIAN_POINT('Ctrl Pts',(10.1999984889428,-1.1967261327477,0.621202329970501));
#11869=CARTESIAN_POINT('Ctrl Pts',(10.1999978161146,-1.19444079525024,0.628767398200536));
#11870=CARTESIAN_POINT('Ctrl Pts',(10.1999974438306,-1.19317629038787,0.632953241898348));
#11871=CARTESIAN_POINT('Ctrl Pts',(10.1999972759003,-1.19164034846853,0.637061602680377));
#11872=CARTESIAN_POINT('Ctrl Pts',(10.1999973648938,-1.18984073583679,0.641063423920242));
#11873=CARTESIAN_POINT('Ctrl Pts',(10.1999975257516,-1.18658789218766,0.648296813248274));
#11874=CARTESIAN_POINT('Ctrl Pts',(10.1999986492083,-1.18251199594868,0.655103972585077));
#11875=CARTESIAN_POINT('Ctrl Pts',(10.1999990866637,-1.1776776067306,0.66132208754656));
#11876=CARTESIAN_POINT('Ctrl Pts',(10.1999991692372,-1.17676507450965,0.662495809810115));
#11877=CARTESIAN_POINT('Ctrl Pts',(10.1999992204458,-1.17582538639523,0.663648473741297));
#11878=CARTESIAN_POINT('Ctrl Pts',(10.1999992199672,-1.17485880188435,0.664778864469789));
#11879=CARTESIAN_POINT('Ctrl Pts',(10.1999992190419,-1.17299032792757,0.666963987046661));
#11880=CARTESIAN_POINT('Ctrl Pts',(10.1999990265713,-1.17102137903347,0.669065925022507));
#11881=CARTESIAN_POINT('Ctrl Pts',(10.1999987631451,-1.16895889720817,0.671081139337088));
#11882=CARTESIAN_POINT('Ctrl Pts',(10.1999980371048,-1.16327440276409,0.676635357771578));
#11883=CARTESIAN_POINT('Ctrl Pts',(10.1999968952367,-1.15694629605269,0.681471105251756));
#11884=CARTESIAN_POINT('Ctrl Pts',(10.1999965193249,-1.15013861030111,0.685534582868085));
#11885=CARTESIAN_POINT('Ctrl Pts',(10.1999962798276,-1.14580136285465,0.688123466749966));
#11886=CARTESIAN_POINT('Ctrl Pts',(10.1999963003895,-1.14126848503633,0.690398200126003));
#11887=CARTESIAN_POINT('Ctrl Pts',(10.1999965837416,-1.13657664085124,0.692335536714198));
#11888=CARTESIAN_POINT('Ctrl Pts',(10.199997026059,-1.12925259320479,0.695359751696499));
#11889=CARTESIAN_POINT('Ctrl Pts',(10.1999981114625,-1.12162598460505,0.697529439192009));
#11890=CARTESIAN_POINT('Ctrl Pts',(10.1999989867727,-1.11384404680861,0.698775198878229));
#11891=CARTESIAN_POINT('Ctrl Pts',(10.1999995533653,-1.10880676031141,0.699581585232154));
#11892=CARTESIAN_POINT('Ctrl Pts',(10.200000000559,-1.10370379302489,0.699999999512891));
#11893=CARTESIAN_POINT('Ctrl Pts',(10.1999999999973,-1.09857320510493,0.7));
#11894=CARTESIAN_POINT('Ctrl Pts',(10.0273290644374,-1.24073895154929,-0.000342977371441382));
#11895=CARTESIAN_POINT('Ctrl Pts',(10.0182194939277,-1.2301570933055,0.201590462913323));
#11896=CARTESIAN_POINT('Ctrl Pts',(10.0091098064739,-1.21957524432673,0.403523898419685));
#11897=CARTESIAN_POINT('Ctrl Pts',(10.,-1.20899340483173,0.605457329065658));
#11898=CARTESIAN_POINT('Ctrl Pts',(9.11786336174441,-1.287320026752,-0.000205293215301774));
#11899=CARTESIAN_POINT('Ctrl Pts',(9.11054075262461,-1.27673792859995,0.201728409731728));
#11900=CARTESIAN_POINT('Ctrl Pts',(9.10321803982027,-1.2661558351744,0.403662109352091));
#11901=CARTESIAN_POINT('Ctrl Pts',(9.09589522044064,-1.25557375159922,0.605595805683776));
#11902=CARTESIAN_POINT('Ctrl Pts',(8.20875307681921,-1.32613868191631,-8.19769783003664E-5));
#11903=CARTESIAN_POINT('Ctrl Pts',(8.20321812688803,-1.31555630757271,0.201851960079368));
#11904=CARTESIAN_POINT('Ctrl Pts',(8.19768309032111,-1.30497393555236,0.403785895133155));
#11905=CARTESIAN_POINT('Ctrl Pts',(8.19214796413157,-1.29439157095064,0.605719828258773));
#11906=CARTESIAN_POINT('Ctrl Pts',(7.29999999999999,-1.35236351479115,1.04083408558608E-17));
#11907=CARTESIAN_POINT('Ctrl Pts',(7.29625341766944,-1.34178092325774,0.201934092022114));
#11908=CARTESIAN_POINT('Ctrl Pts',(7.2925067690755,-1.33119833465137,0.403868182971915));
#11909=CARTESIAN_POINT('Ctrl Pts',(7.28876005303739,-1.32061574904145,0.605802272831199));
#11910=CARTESIAN_POINT('Ctrl Pts',(7.29999999953094,-1.32031613471704,0.605285370449856));
#11911=CARTESIAN_POINT('Ctrl Pts',(8.20058408060299,-1.29406305600824,0.605326635812744));
#11912=CARTESIAN_POINT('Ctrl Pts',(9.10058974048747,-1.25534320916473,0.605388449123016));
#11913=CARTESIAN_POINT('Ctrl Pts',(9.99999999968202,-1.20899340489109,0.605457329065633));
#11914=CARTESIAN_POINT('Ctrl Pts',(10.5052670937641,-1.21555282972197,-4.72190879230918E-5));
#11915=CARTESIAN_POINT('Ctrl Pts',(10.4952228315222,-1.20497561405085,0.201799837144789));
#11916=CARTESIAN_POINT('Ctrl Pts',(10.4851784461209,-1.19439840869387,0.403646887802288));
#11917=CARTESIAN_POINT('Ctrl Pts',(10.4751339353761,-1.18382121389426,0.605493932788863));
#11918=CARTESIAN_POINT('Ctrl Pts',(10.4035069533234,-1.22105168617584,-3.13467776074076E-5));
#11919=CARTESIAN_POINT('Ctrl Pts',(10.3936624949941,-1.21047444506522,0.201815739766394));
#11920=CARTESIAN_POINT('Ctrl Pts',(10.3838179147697,-1.19989721405033,0.403662820908308));
#11921=CARTESIAN_POINT('Ctrl Pts',(10.3739732104882,-1.18931999337004,0.605509896555428));
#11922=CARTESIAN_POINT('Ctrl Pts',(10.3017512542637,-1.22646400658821,-1.55943981238903E-5));
#11923=CARTESIAN_POINT('Ctrl Pts',(10.2921066085356,-1.21588673949083,0.201831522212972));
#11924=CARTESIAN_POINT('Ctrl Pts',(10.2824618422276,-1.20530948226626,0.403678633593635));
#11925=CARTESIAN_POINT('Ctrl Pts',(10.2728169532007,-1.19473223514815,0.605525739654126));
#11926=CARTESIAN_POINT('Ctrl Pts',(10.2,-1.23178301601145,-4.5102810375397E-17));
#11927=CARTESIAN_POINT('Ctrl Pts',(10.1905551755811,-1.22120572247414,0.20184714636246));
#11928=CARTESIAN_POINT('Ctrl Pts',(10.1811102319487,-1.21062843858304,0.403694287664275));
#11929=CARTESIAN_POINT('Ctrl Pts',(10.1716651669877,-1.20005116456574,0.605541423818621));
#11930=CARTESIAN_POINT('',(10.4735630903435,-1.18390659316268,0.605494180667944));
#11931=CARTESIAN_POINT('Ctrl Pts',(10.1999999975038,-1.19856231440453,0.605472757505366));
#11932=CARTESIAN_POINT('Ctrl Pts',(10.2911933328565,-1.19375025772558,0.605479840815741));
#11933=CARTESIAN_POINT('Ctrl Pts',(10.3823809652617,-1.18886335120032,0.605486986548286));
#11934=CARTESIAN_POINT('Ctrl Pts',(10.4735630903435,-1.18390659316268,0.605494180667944));
#11935=CARTESIAN_POINT('Ctrl Pts',(10.4735630903435,-1.18390659316268,0.605494180667945));
#11936=CARTESIAN_POINT('Ctrl Pts',(10.4841302498201,-1.19445434834508,0.403662775875149));
#11937=CARTESIAN_POINT('Ctrl Pts',(10.4946974680575,-1.20500226999407,0.201831382381129));
#11938=CARTESIAN_POINT('Ctrl Pts',(10.5052647440597,-1.21555035534119,-6.86299975183324E-17));
#11939=CARTESIAN_POINT('Ctrl Pts',(10.,-1.10900986674273,0.7));
#11940=CARTESIAN_POINT('Ctrl Pts',(9.09944331332257,-1.15544418981837,0.7));
#11941=CARTESIAN_POINT('Ctrl Pts',(8.1984670949788,-1.19422430779862,0.7));
#11942=CARTESIAN_POINT('Ctrl Pts',(7.29709043526679,-1.22049830417059,0.7));
#11943=CARTESIAN_POINT('Ctrl Pts',(10.0014871213396,-1.13785139984992,0.7));
#11944=CARTESIAN_POINT('Ctrl Pts',(9.10076698492608,-1.18430758604571,0.700000491839571));
#11945=CARTESIAN_POINT('Ctrl Pts',(8.19957769811723,-1.22310890030201,0.699999704549177));
#11946=CARTESIAN_POINT('Ctrl Pts',(7.29793284700475,-1.24939875264889,0.7));
#11947=CARTESIAN_POINT('Ctrl Pts',(10.0040646682326,-1.18784086746588,0.676686753673613));
#11948=CARTESIAN_POINT('Ctrl Pts',(9.10306300621911,-1.23433322993607,0.676664155483858));
#11949=CARTESIAN_POINT('Ctrl Pts',(8.20149954052229,-1.27317186922949,0.676644146017133));
#11950=CARTESIAN_POINT('Ctrl Pts',(7.29939288958795,-1.29948813715084,0.676630595533454));
#11951=CARTESIAN_POINT('Ctrl Pts',(10.0050807923581,-1.20754778500352,0.627085325222079));
#11952=CARTESIAN_POINT('Ctrl Pts',(9.10396596140607,-1.25402923300358,0.627026849623412));
#11953=CARTESIAN_POINT('Ctrl Pts',(8.20225661204673,-1.29285896783792,0.626974637782525));
#11954=CARTESIAN_POINT('Ctrl Pts',(7.29996660609514,-1.31917051289423,0.626939603849942));
#11955=CARTESIAN_POINT('Ctrl Pts',(10.0051416645797,-1.20872835322339,0.605457722909465));
#11956=CARTESIAN_POINT('Ctrl Pts',(9.1040197884667,-1.25519559703033,0.605388684776982));
#11957=CARTESIAN_POINT('Ctrl Pts',(8.20230020786566,-1.29401302889245,0.605326714446839));
#11958=CARTESIAN_POINT('Ctrl Pts',(7.29999999953094,-1.32031613471704,0.605285370449856));
#11959=CARTESIAN_POINT('Ctrl Pts',(10.4681436286308,-1.08420482079362,0.7));
#11960=CARTESIAN_POINT('Ctrl Pts',(10.3770124662346,-1.0891584122264,0.7));
#11961=CARTESIAN_POINT('Ctrl Pts',(10.285877616441,-1.09404209584202,0.7));
#11962=CARTESIAN_POINT('Ctrl Pts',(10.1947388861048,-1.09885088260188,0.7));
#11963=CARTESIAN_POINT('Ctrl Pts',(10.4697107510168,-1.11303515260326,0.7));
#11964=CARTESIAN_POINT('Ctrl Pts',(10.3785648662465,-1.11799094453753,0.700000051218742));
#11965=CARTESIAN_POINT('Ctrl Pts',(10.2874149314686,-1.12287675076168,0.699999949550842));
#11966=CARTESIAN_POINT('Ctrl Pts',(10.196260416419,-1.12768774893097,0.7));
#11967=CARTESIAN_POINT('Ctrl Pts',(10.4724269697127,-1.16300539549315,0.676698381019543));
#11968=CARTESIAN_POINT('Ctrl Pts',(10.3812557252598,-1.16796482352885,0.676696026813929));
#11969=CARTESIAN_POINT('Ctrl Pts',(10.2900793016129,-1.17285439035486,0.676693724638983));
#11970=CARTESIAN_POINT('Ctrl Pts',(10.1988975981852,-1.17766904563614,0.67669140632491));
#11971=CARTESIAN_POINT('Ctrl Pts',(10.4734985149421,-1.18271860027509,0.627116141711795));
#11972=CARTESIAN_POINT('Ctrl Pts',(10.382317043787,-1.18767684023183,0.627110048826767));
#11973=CARTESIAN_POINT('Ctrl Pts',(10.2911301919381,-1.19256517083271,0.627104033151799));
#11974=CARTESIAN_POINT('Ctrl Pts',(10.1999375452555,-1.19737868557977,0.627098033786781));
#11975=CARTESIAN_POINT('Ctrl Pts',(10.4735630903435,-1.18390659316268,0.605494180667944));
#11976=CARTESIAN_POINT('Ctrl Pts',(10.3823809652617,-1.18886335120032,0.605486986548286));
#11977=CARTESIAN_POINT('Ctrl Pts',(10.2911933328565,-1.19375025772558,0.605479840815741));
#11978=CARTESIAN_POINT('Ctrl Pts',(10.1999999975038,-1.19856231440453,0.605472757505366));
#11979=CARTESIAN_POINT('',(10.4681436258201,-1.08420482094639,0.7));
#11980=CARTESIAN_POINT('Ctrl Pts',(10.4681436258201,-1.0842048209464,0.7));
#11981=CARTESIAN_POINT('Ctrl Pts',(10.3787660248044,-1.08906309452597,0.7));
#11982=CARTESIAN_POINT('Ctrl Pts',(10.289384876933,-1.09385412476048,0.7));
#11983=CARTESIAN_POINT('Ctrl Pts',(10.1999999999973,-1.09857320510493,0.7));
#11984=CARTESIAN_POINT('Origin',(10.4681436286308,-1.08420482099672,0.6));
#11985=CARTESIAN_POINT('Origin',(5.4,-8.11656130105013E-18,0.7));
#11986=CARTESIAN_POINT('',(10.4681436286308,1.08420482109828,0.7));
#11987=CARTESIAN_POINT('Ctrl Pts',(10.1999999980461,1.09857320520795,0.7));
#11988=CARTESIAN_POINT('Ctrl Pts',(10.2893848765692,1.09385412478074,0.7));
#11989=CARTESIAN_POINT('Ctrl Pts',(10.3787660260279,1.08906309446088,0.7));
#11990=CARTESIAN_POINT('Ctrl Pts',(10.4681436286308,1.08420482079361,0.7));
#11991=CARTESIAN_POINT('',(10.4681436286308,0.7,0.7));
#11992=CARTESIAN_POINT('Ctrl Pts',(7.3,1.35236351479305,-3.57463069561303E-11));
#11993=CARTESIAN_POINT('Ctrl Pts',(7.29625341766908,1.34178092325856,0.20193409200674));
#11994=CARTESIAN_POINT('Ctrl Pts',(7.29250676907475,1.33119833465113,0.403868182976914));
#11995=CARTESIAN_POINT('Ctrl Pts',(7.28876005303626,1.32061574904014,0.60580227285657));
#11996=CARTESIAN_POINT('Ctrl Pts',(8.20875307682014,1.32613868191819,-8.19770140467192E-5));
#11997=CARTESIAN_POINT('Ctrl Pts',(8.20321812688841,1.31555630757352,0.201851960063995));
#11998=CARTESIAN_POINT('Ctrl Pts',(8.19768309032092,1.3049739355521,0.403785895138154));
#11999=CARTESIAN_POINT('Ctrl Pts',(8.19214796413082,1.29439157094932,0.605719828284144));
#12000=CARTESIAN_POINT('Ctrl Pts',(9.11786336174626,1.28732002675385,-0.000205293251048056));
#12001=CARTESIAN_POINT('Ctrl Pts',(9.11054075262572,1.27673792860073,0.201728409716354));
#12002=CARTESIAN_POINT('Ctrl Pts',(9.10321803982063,1.26615583517412,0.403662109357089));
#12003=CARTESIAN_POINT('Ctrl Pts',(9.09589522044026,1.25557375159787,0.605595805709147));
#12004=CARTESIAN_POINT('Ctrl Pts',(10.0273290644402,1.2407389515511,-0.000342977407187712));
#12005=CARTESIAN_POINT('Ctrl Pts',(10.0182194939295,1.23015709330624,0.201590462897949));
#12006=CARTESIAN_POINT('Ctrl Pts',(10.0091098064748,1.21957524432641,0.403523898424684));
#12007=CARTESIAN_POINT('Ctrl Pts',(10.,1.20899340483035,0.605457329091028));
#12008=CARTESIAN_POINT('Ctrl Pts',(10.2,1.23178301601276,-2.39624899783797E-11));
#12009=CARTESIAN_POINT('Ctrl Pts',(10.1905551755807,1.22120572247504,0.201847146346486));
#12010=CARTESIAN_POINT('Ctrl Pts',(10.1811102319479,1.21062843858352,0.403694287656288));
#12011=CARTESIAN_POINT('Ctrl Pts',(10.1716651669865,1.2000511645658,0.605541423818621));
#12012=CARTESIAN_POINT('Ctrl Pts',(10.3017512542641,1.22646400658951,-1.55944220863836E-5));
#12013=CARTESIAN_POINT('Ctrl Pts',(10.2921066085356,1.2158867394917,0.201831522196997));
#12014=CARTESIAN_POINT('Ctrl Pts',(10.2824618422272,1.20530948226672,0.403678633585648));
#12015=CARTESIAN_POINT('Ctrl Pts',(10.2728169531999,1.19473223514819,0.605525739654127));
#12016=CARTESIAN_POINT('Ctrl Pts',(10.4035069533242,1.22105168617711,-3.13468015701665E-5));
#12017=CARTESIAN_POINT('Ctrl Pts',(10.3936624949945,1.21047444506608,0.201815739750419));
#12018=CARTESIAN_POINT('Ctrl Pts',(10.3838179147698,1.19989721405077,0.40366282090032));
#12019=CARTESIAN_POINT('Ctrl Pts',(10.3739732104878,1.18931999337006,0.605509896555428));
#12020=CARTESIAN_POINT('Ctrl Pts',(10.5052670937653,1.21555282972323,-4.72191118859062E-5));
#12021=CARTESIAN_POINT('Ctrl Pts',(10.495222831523,1.20497561405169,0.201799837128814));
#12022=CARTESIAN_POINT('Ctrl Pts',(10.4851784461213,1.19439840869429,0.403646887794301));
#12023=CARTESIAN_POINT('Ctrl Pts',(10.4751339353761,1.18382121389426,0.605493932788864));
#12024=CARTESIAN_POINT('',(10.4735630903435,1.18390659316268,0.605494180667944));
#12025=CARTESIAN_POINT('Ctrl Pts',(10.5052647440597,1.21555035534119,-4.0462425077159E-16));
#12026=CARTESIAN_POINT('Ctrl Pts',(10.4946974680575,1.20500226999407,0.201831382381129));
#12027=CARTESIAN_POINT('Ctrl Pts',(10.4841302498201,1.19445434834508,0.40366277587515));
#12028=CARTESIAN_POINT('Ctrl Pts',(10.4735630903435,1.18390659316268,0.605494180667945));
#12029=CARTESIAN_POINT('Ctrl Pts',(10.4735630903435,1.18390659316268,0.605494180667944));
#12030=CARTESIAN_POINT('Ctrl Pts',(10.3823809652617,1.18886335120032,0.605486986548286));
#12031=CARTESIAN_POINT('Ctrl Pts',(10.2911933328565,1.19375025772558,0.605479840815741));
#12032=CARTESIAN_POINT('Ctrl Pts',(10.1999999975038,1.19856231440453,0.605472757505366));
#12033=CARTESIAN_POINT('Origin',(7.1,1.42555555555556,0.));
#12034=CARTESIAN_POINT('',(7.0999999994629,-1.32593912634735,0.605276549957215));
#12035=CARTESIAN_POINT('Ctrl Pts',(7.0999999994629,-1.32593912634735,0.605276549957215));
#12036=CARTESIAN_POINT('Ctrl Pts',(7.0999999994629,-1.33126650931098,0.504490734647167));
#12037=CARTESIAN_POINT('Ctrl Pts',(7.1,-1.33659376385849,0.403703958452373));
#12038=CARTESIAN_POINT('Ctrl Pts',(7.1,-1.3472576786761,0.201945747207886));
#12039=CARTESIAN_POINT('Ctrl Pts',(7.1,-1.35259443928223,0.100972400854069));
#12040=CARTESIAN_POINT('Ctrl Pts',(7.1,-1.35793097395724,0.));
#12041=CARTESIAN_POINT('',(7.1,-1.22604182196417,0.7));
#12042=CARTESIAN_POINT('Ctrl Pts',(7.1,-1.22604182196307,0.7));
#12043=CARTESIAN_POINT('Ctrl Pts',(7.1,-1.23395163718705,0.7));
#12044=CARTESIAN_POINT('Ctrl Pts',(7.09999945440688,-1.24179783218049,0.699006056038995));
#12045=CARTESIAN_POINT('Ctrl Pts',(7.09999897931553,-1.2494401870438,0.697119011207626));
#12046=CARTESIAN_POINT('Ctrl Pts',(7.09999871186578,-1.25374240366384,0.696056710937424));
#12047=CARTESIAN_POINT('Ctrl Pts',(7.09999846845149,-1.25798007942473,0.69471034534287));
#12048=CARTESIAN_POINT('Ctrl Pts',(7.09999831430822,-1.26212651101681,0.6930909329195));
#12049=CARTESIAN_POINT('Ctrl Pts',(7.09999803835695,-1.26954956016987,0.690191818885951));
#12050=CARTESIAN_POINT('Ctrl Pts',(7.09999810102228,-1.27659977900265,0.686452252582521));
#12051=CARTESIAN_POINT('Ctrl Pts',(7.09999845706054,-1.28313109767173,0.681953977461377));
#12052=CARTESIAN_POINT('Ctrl Pts',(7.09999865314126,-1.2867280867584,0.679476645189077));
#12053=CARTESIAN_POINT('Ctrl Pts',(7.09999893113315,-1.29016742765117,0.67676830886676));
#12054=CARTESIAN_POINT('Ctrl Pts',(7.09999917787259,-1.2934208019838,0.673837071833988));
#12055=CARTESIAN_POINT('Ctrl Pts',(7.09999941835505,-1.29659167515528,0.670980166997299));
#12056=CARTESIAN_POINT('Ctrl Pts',(7.09999963169439,-1.29956664557352,0.667928795646746));
#12057=CARTESIAN_POINT('Ctrl Pts',(7.09999963110542,-1.30232317314677,0.664694459428825));
#12058=CARTESIAN_POINT('Ctrl Pts',(7.09999963001387,-1.30743194453681,0.658700148145236));
#12059=CARTESIAN_POINT('Ctrl Pts',(7.09999897381858,-1.31179333085743,0.652078782729069));
#12060=CARTESIAN_POINT('Ctrl Pts',(7.09999874753952,-1.31534789998199,0.64499600756552));
#12061=CARTESIAN_POINT('Ctrl Pts',(7.09999872438549,-1.31571162172319,0.644271261689237));
#12062=CARTESIAN_POINT('Ctrl Pts',(7.0999987046402,-1.31606685549941,0.643541664816448));
#12063=CARTESIAN_POINT('Ctrl Pts',(7.09999868869212,-1.31641350913238,0.642807383257706));
#12064=CARTESIAN_POINT('Ctrl Pts',(7.09999853283271,-1.31980133087414,0.635631300872562));
#12065=CARTESIAN_POINT('Ctrl Pts',(7.09999885939544,-1.32233451509485,0.628092322434426));
#12066=CARTESIAN_POINT('Ctrl Pts',(7.09999934101855,-1.32395982399511,0.620358959365968));
#12067=CARTESIAN_POINT('Ctrl Pts',(7.09999964997549,-1.32500244522074,0.615398075635307));
#12068=CARTESIAN_POINT('Ctrl Pts',(7.09999999934316,-1.32567060646853,0.610356529630438));
#12069=CARTESIAN_POINT('Ctrl Pts',(7.09999999981141,-1.32593912630714,0.60527654995744));
#12070=CARTESIAN_POINT('',(7.09999999995537,1.22604182196549,0.7));
#12071=CARTESIAN_POINT('',(7.1,0.712777777777778,0.7));
#12072=CARTESIAN_POINT('',(7.0999999994629,1.32593912634735,0.605276549957215));
#12073=CARTESIAN_POINT('Ctrl Pts',(7.09999999981142,1.32593912630714,0.60527654995744));
#12074=CARTESIAN_POINT('Ctrl Pts',(7.09999999908198,1.32552083177145,0.613190035045322));
#12075=CARTESIAN_POINT('Ctrl Pts',(7.09999922367565,1.32413525001942,0.621012727860624));
#12076=CARTESIAN_POINT('Ctrl Pts',(7.09999888117586,1.32186630199077,0.628584136488803));
#12077=CARTESIAN_POINT('Ctrl Pts',(7.09999868987568,1.32059900146923,0.632813078704371));
#12078=CARTESIAN_POINT('Ctrl Pts',(7.09999860640034,1.3190551184949,0.636963663611311));
#12079=CARTESIAN_POINT('Ctrl Pts',(7.09999865766138,1.31724253497577,0.641005923298765));
#12080=CARTESIAN_POINT('Ctrl Pts',(7.0999987494091,1.31399834762864,0.648240816253195));
#12081=CARTESIAN_POINT('Ctrl Pts',(7.09999933613984,1.30993159792479,0.655050690394837));
#12082=CARTESIAN_POINT('Ctrl Pts',(7.09999956222935,1.30510592187917,0.661272231165006));
#12083=CARTESIAN_POINT('Ctrl Pts',(7.09999960444598,1.30420484616769,0.662433950108221));
#12084=CARTESIAN_POINT('Ctrl Pts',(7.09999963060969,1.30327718139331,0.663575086117144));
#12085=CARTESIAN_POINT('Ctrl Pts',(7.09999963056866,1.30232317316131,0.664694459428815));
#12086=CARTESIAN_POINT('Ctrl Pts',(7.09999963048683,1.30042028596585,0.666927187690779));
#12087=CARTESIAN_POINT('Ctrl Pts',(7.09999952705857,1.29841262431024,0.669073382394206));
#12088=CARTESIAN_POINT('Ctrl Pts',(7.09999938633452,1.29630755303174,0.671129253595323));
#12089=CARTESIAN_POINT('Ctrl Pts',(7.09999900634735,1.29062337821964,0.676680576924663));
#12090=CARTESIAN_POINT('Ctrl Pts',(7.09999841760642,1.2842958957007,0.681513596217188));
#12091=CARTESIAN_POINT('Ctrl Pts',(7.0999982224057,1.2774887935492,0.68557385059291));
#12092=CARTESIAN_POINT('Ctrl Pts',(7.09999809840912,1.27316474526651,0.688153029745784));
#12093=CARTESIAN_POINT('Ctrl Pts',(7.09999810738417,1.26864620899217,0.690419707112974));
#12094=CARTESIAN_POINT('Ctrl Pts',(7.09999825155258,1.26396949224645,0.69235064530212));
#12095=CARTESIAN_POINT('Ctrl Pts',(7.09999847710269,1.25665281355793,0.695371579659609));
#12096=CARTESIAN_POINT('Ctrl Pts',(7.09999903441007,1.2490339950321,0.697538299034574));
#12097=CARTESIAN_POINT('Ctrl Pts',(7.09999948258254,1.24125996729125,0.698781081437474));
#12098=CARTESIAN_POINT('Ctrl Pts',(7.09999977198436,1.23623998534067,0.699583592753232));
#12099=CARTESIAN_POINT('Ctrl Pts',(7.1,1.23115469319345,0.7));
#12100=CARTESIAN_POINT('Ctrl Pts',(7.1,1.22604182196307,0.7));
#12101=CARTESIAN_POINT('Ctrl Pts',(7.1,1.35793097395724,0.));
#12102=CARTESIAN_POINT('Ctrl Pts',(7.1,1.35259441576718,0.100972845781549));
#12103=CARTESIAN_POINT('Ctrl Pts',(7.1,1.34725763161617,0.201946637598055));
#12104=CARTESIAN_POINT('Ctrl Pts',(7.1,1.33659371676552,0.403704849408333));
#12105=CARTESIAN_POINT('Ctrl Pts',(7.0999999994629,1.33126648576411,0.504491180117376));
#12106=CARTESIAN_POINT('Ctrl Pts',(7.0999999994629,1.32593912634735,0.605276549957215));
#12107=CARTESIAN_POINT('Ctrl Pts',(7.11011156210589,-1.35766432821499,-9.27062925672982E-5));
#12108=CARTESIAN_POINT('Ctrl Pts',(7.10674110347764,-1.34708925835705,0.201697046690488));
#12109=CARTESIAN_POINT('Ctrl Pts',(7.10337058314201,-1.33651419103807,0.403486798779133));
#12110=CARTESIAN_POINT('Ctrl Pts',(7.09999999999996,-1.32593912631822,0.605276549958221));
#12111=CARTESIAN_POINT('Ctrl Pts',(5.9694837631095,-1.38835096090528,2.80675674898241E-6));
#12112=CARTESIAN_POINT('Ctrl Pts',(5.96835662351021,-1.37777563343505,0.201792740207853));
#12113=CARTESIAN_POINT('Ctrl Pts',(5.96722945517891,-1.3672003004237,0.40358267322573));
#12114=CARTESIAN_POINT('Ctrl Pts',(5.96610224583462,-1.35662497356325,0.605372606931572));
#12115=CARTESIAN_POINT('Ctrl Pts',(4.8294200007394,-1.39866452387306,3.01102374082134E-5));
#12116=CARTESIAN_POINT('Ctrl Pts',(4.83053730380309,-1.38808904115766,0.201820093264151));
#12117=CARTESIAN_POINT('Ctrl Pts',(4.83165461298617,-1.3775135517806,0.403610075973038));
#12118=CARTESIAN_POINT('Ctrl Pts',(4.83277191472125,-1.36693806692183,0.605400059795761));
#12119=CARTESIAN_POINT('Ctrl Pts',(3.68991216363982,-1.37907703205181,-6.2684699445455E-5));
#12120=CARTESIAN_POINT('Ctrl Pts',(3.69327498756969,-1.36850179198701,0.201727122618256));
#12121=CARTESIAN_POINT('Ctrl Pts',(3.69663785098144,-1.3579265529724,0.403516929334346));
#12122=CARTESIAN_POINT('Ctrl Pts',(3.70000075457889,-1.34735131503281,0.605306735438421));
#12123=CARTESIAN_POINT('Ctrl Pts',(3.69999999992215,-1.34735368792773,0.6052614572053));
#12124=CARTESIAN_POINT('Ctrl Pts',(4.83355316856959,-1.366961322855,0.605214762857233));
#12125=CARTESIAN_POINT('Ctrl Pts',(5.96724522208681,-1.35660163688233,0.605228569880684));
#12126=CARTESIAN_POINT('Ctrl Pts',(7.09999999927392,-1.32593912632169,0.605276549957417));
#12127=CARTESIAN_POINT('Ctrl Pts',(7.1,-1.22604182196307,0.7));
#12128=CARTESIAN_POINT('Ctrl Pts',(5.96696284938742,-1.25674179781664,0.7));
#12129=CARTESIAN_POINT('Ctrl Pts',(4.83327074934872,-1.26710800714677,0.7));
#12130=CARTESIAN_POINT('Ctrl Pts',(3.7,-1.24747724070879,0.7));
#12131=CARTESIAN_POINT('Ctrl Pts',(7.10078315634008,-1.25494559805327,0.7));
#12132=CARTESIAN_POINT('Ctrl Pts',(5.96739926106349,-1.28566432005869,0.700000343763215));
#12133=CARTESIAN_POINT('Ctrl Pts',(4.83328164159484,-1.29603890521481,0.700000334703603));
#12134=CARTESIAN_POINT('Ctrl Pts',(3.69949916377151,-1.27639017438114,0.7));
#12135=CARTESIAN_POINT('Ctrl Pts',(7.10214055788579,-1.30504291366416,0.676629771601708));
#12136=CARTESIAN_POINT('Ctrl Pts',(5.96815960929481,-1.33579288254824,0.676614006760374));
#12137=CARTESIAN_POINT('Ctrl Pts',(4.83329467960724,-1.3461818279488,0.676609489640654));
#12138=CARTESIAN_POINT('Ctrl Pts',(3.69863109538965,-1.3265031696486,0.676624836591801));
#12139=CARTESIAN_POINT('Ctrl Pts',(7.10267376869946,-1.32472200604796,0.626932241521275));
#12140=CARTESIAN_POINT('Ctrl Pts',(5.9684558952243,-1.35546668061705,0.626891484245174));
#12141=CARTESIAN_POINT('Ctrl Pts',(4.83330292199863,-1.36585610284781,0.626879766983475));
#12142=CARTESIAN_POINT('Ctrl Pts',(3.69829020046733,-1.34618280086838,0.626919440930842));
#12143=CARTESIAN_POINT('Ctrl Pts',(7.10270476209941,-1.32586587253612,0.605276664588022));
#12144=CARTESIAN_POINT('Ctrl Pts',(5.96847377630401,-1.35660073810322,0.605228567467576));
#12145=CARTESIAN_POINT('Ctrl Pts',(4.8333022084086,-1.36698748587873,0.605214711607465));
#12146=CARTESIAN_POINT('Ctrl Pts',(3.69827043673666,-1.34732374755196,0.60526152849799));
#12147=CARTESIAN_POINT('Ctrl Pts',(7.1,-1.22604182196307,0.7));
#12148=CARTESIAN_POINT('Ctrl Pts',(5.96696284938742,-1.25674179781664,0.7));
#12149=CARTESIAN_POINT('Ctrl Pts',(4.83327074934872,-1.26710800714677,0.7));
#12150=CARTESIAN_POINT('Ctrl Pts',(3.7,-1.24747724070879,0.7));
#12151=CARTESIAN_POINT('Origin',(5.4,-8.11656130105013E-18,0.7));
#12152=CARTESIAN_POINT('Ctrl Pts',(3.7,1.24747724070879,0.7));
#12153=CARTESIAN_POINT('Ctrl Pts',(4.83327074934871,1.26710800714677,0.7));
#12154=CARTESIAN_POINT('Ctrl Pts',(5.96696284938742,1.25674179781664,0.7));
#12155=CARTESIAN_POINT('Ctrl Pts',(7.1,1.22604182196307,0.7));
#12156=CARTESIAN_POINT('Ctrl Pts',(3.7,1.24747724070879,0.7));
#12157=CARTESIAN_POINT('Ctrl Pts',(4.83327074934871,1.26710800714677,0.7));
#12158=CARTESIAN_POINT('Ctrl Pts',(5.96696284938742,1.25674179781664,0.7));
#12159=CARTESIAN_POINT('Ctrl Pts',(7.1,1.22604182196307,0.7));
#12160=CARTESIAN_POINT('Ctrl Pts',(3.69949916377151,1.27639017438114,0.7));
#12161=CARTESIAN_POINT('Ctrl Pts',(4.83328164159484,1.29603890521481,0.700000334703603));
#12162=CARTESIAN_POINT('Ctrl Pts',(5.96739926106349,1.28566432005869,0.700000343763215));
#12163=CARTESIAN_POINT('Ctrl Pts',(7.10078315634008,1.25494559805327,0.7));
#12164=CARTESIAN_POINT('Ctrl Pts',(3.69863109538965,1.3265031696486,0.676624836591801));
#12165=CARTESIAN_POINT('Ctrl Pts',(4.83329467960724,1.3461818279488,0.676609489640654));
#12166=CARTESIAN_POINT('Ctrl Pts',(5.9681596092948,1.33579288254824,0.676614006760374));
#12167=CARTESIAN_POINT('Ctrl Pts',(7.10214055788579,1.30504291366416,0.676629771601707));
#12168=CARTESIAN_POINT('Ctrl Pts',(3.69829020046733,1.34618280086838,0.626919440930842));
#12169=CARTESIAN_POINT('Ctrl Pts',(4.83330292199863,1.36585610284781,0.626879766983475));
#12170=CARTESIAN_POINT('Ctrl Pts',(5.9684558952243,1.35546668061705,0.626891484245174));
#12171=CARTESIAN_POINT('Ctrl Pts',(7.10267376869946,1.32472200604796,0.626932241521275));
#12172=CARTESIAN_POINT('Ctrl Pts',(3.69827043673666,1.34732374755196,0.60526152849799));
#12173=CARTESIAN_POINT('Ctrl Pts',(4.83330220840859,1.36698748587873,0.605214711607465));
#12174=CARTESIAN_POINT('Ctrl Pts',(5.96847377630401,1.35660073810322,0.605228567467576));
#12175=CARTESIAN_POINT('Ctrl Pts',(7.10270476209941,1.32586587253612,0.605276664588022));
#12176=CARTESIAN_POINT('Ctrl Pts',(7.09999999927392,1.32593912632169,0.605276549957417));
#12177=CARTESIAN_POINT('Ctrl Pts',(5.96724522208681,1.35660163688233,0.605228569880684));
#12178=CARTESIAN_POINT('Ctrl Pts',(4.83355316856959,1.366961322855,0.605214762857233));
#12179=CARTESIAN_POINT('Ctrl Pts',(3.69999999992215,1.34735368792773,0.6052614572053));
#12180=CARTESIAN_POINT('Ctrl Pts',(3.68991216360307,1.37907703216746,-6.26869063400631E-5));
#12181=CARTESIAN_POINT('Ctrl Pts',(3.6932749875452,1.36850179206412,0.201727121146993));
#12182=CARTESIAN_POINT('Ctrl Pts',(3.69663785096921,1.35792655301095,0.403516928598715));
#12183=CARTESIAN_POINT('Ctrl Pts',(3.70000075457892,1.34735131503281,0.605306735438421));
#12184=CARTESIAN_POINT('Ctrl Pts',(4.8294200007272,1.39866452398872,3.01080305115927E-5));
#12185=CARTESIAN_POINT('Ctrl Pts',(4.83053730379496,1.38808904123477,0.201820091792887));
#12186=CARTESIAN_POINT('Ctrl Pts',(4.83165461298211,1.37751355181915,0.403610075237406));
#12187=CARTESIAN_POINT('Ctrl Pts',(4.83277191472127,1.36693806692183,0.605400059795761));
#12188=CARTESIAN_POINT('Ctrl Pts',(5.96948376312183,1.38835096102094,2.80454985295556E-6));
#12189=CARTESIAN_POINT('Ctrl Pts',(5.96835662351844,1.37777563351215,0.201792738736588));
#12190=CARTESIAN_POINT('Ctrl Pts',(5.96722945518303,1.36720030046225,0.403582672490098));
#12191=CARTESIAN_POINT('Ctrl Pts',(5.96610224583462,1.35662497356325,0.605372606931572));
#12192=CARTESIAN_POINT('Ctrl Pts',(7.11011156214274,1.35766432833065,-9.27084994613511E-5));
#12193=CARTESIAN_POINT('Ctrl Pts',(7.10674110350221,1.34708925843416,0.201697045219225));
#12194=CARTESIAN_POINT('Ctrl Pts',(7.10337058315429,1.33651419107662,0.403486798043502));
#12195=CARTESIAN_POINT('Ctrl Pts',(7.09999999999996,1.32593912631822,0.605276549958221));
#12196=CARTESIAN_POINT('Origin',(3.5,1.44777777777778,0.));
#12197=CARTESIAN_POINT('',(3.5,-1.34358136363184,0.605270327458634));
#12198=CARTESIAN_POINT('Ctrl Pts',(3.5,-1.34358136363184,0.605270327458634));
#12199=CARTESIAN_POINT('Ctrl Pts',(3.5,-1.34890136370362,0.504489156176152));
#12200=CARTESIAN_POINT('Ctrl Pts',(3.5,-1.35422123464986,0.403706701640381));
#12201=CARTESIAN_POINT('Ctrl Pts',(3.5,-1.3648706701715,0.201950780690867));
#12202=CARTESIAN_POINT('Ctrl Pts',(3.5,-1.3702003690246,0.100974756199658));
#12203=CARTESIAN_POINT('Ctrl Pts',(3.5,-1.37552980833516,0.));
#12204=CARTESIAN_POINT('',(3.5,-1.24369946473884,0.7));
#12205=CARTESIAN_POINT('Ctrl Pts',(3.49999999991873,-1.24369946470729,0.7));
#12206=CARTESIAN_POINT('Ctrl Pts',(3.49999999896975,-1.25160831520001,0.699999999810925));
#12207=CARTESIAN_POINT('Ctrl Pts',(3.50000040534574,-1.25945374057332,0.69900619751828));
#12208=CARTESIAN_POINT('Ctrl Pts',(3.50000075715473,-1.26709539726361,0.697119355224275));
#12209=CARTESIAN_POINT('Ctrl Pts',(3.5000009551612,-1.27139630362835,0.696057395447694));
#12210=CARTESIAN_POINT('Ctrl Pts',(3.50000113454144,-1.27563271975905,0.694711510656402));
#12211=CARTESIAN_POINT('Ctrl Pts',(3.50000124621709,-1.27977793997275,0.693092697679401));
#12212=CARTESIAN_POINT('Ctrl Pts',(3.50000144618968,-1.28720060051191,0.690193961644836));
#12213=CARTESIAN_POINT('Ctrl Pts',(3.50000138985083,-1.29425038514255,0.686454755369034));
#12214=CARTESIAN_POINT('Ctrl Pts',(3.5000011147959,-1.30078112659466,0.681956784255818));
#12215=CARTESIAN_POINT('Ctrl Pts',(3.50000096334461,-1.30437709646577,0.679480102439082));
#12216=CARTESIAN_POINT('Ctrl Pts',(3.50000075087427,-1.30781543681835,0.676772489296601));
#12217=CARTESIAN_POINT('Ctrl Pts',(3.50000056308077,-1.31106783354026,0.67384203444854));
#12218=CARTESIAN_POINT('Ctrl Pts',(3.50000037990614,-1.31424023611357,0.670983655445047));
#12219=CARTESIAN_POINT('Ctrl Pts',(3.50000021841608,-1.31721646102264,0.667930553458483));
#12220=CARTESIAN_POINT('Ctrl Pts',(3.50000022028926,-1.3199739184757,0.664694242102541));
#12221=CARTESIAN_POINT('Ctrl Pts',(3.50000022375892,-1.32508151834405,0.658699667848218));
#12222=CARTESIAN_POINT('Ctrl Pts',(3.50000072745304,-1.32944146850927,0.652077914129702));
#12223=CARTESIAN_POINT('Ctrl Pts',(3.50000090782832,-1.33299465793893,0.64499486611401));
#12224=CARTESIAN_POINT('Ctrl Pts',(3.50000092626355,-1.33335781125732,0.644270944003422));
#12225=CARTESIAN_POINT('Ctrl Pts',(3.50000094214549,-1.33371249714824,0.643542183465449));
#12226=CARTESIAN_POINT('Ctrl Pts',(3.5000009551778,-1.33405862411533,0.642808750463418));
#12227=CARTESIAN_POINT('Ctrl Pts',(3.50000108270827,-1.3374457225345,0.635631587173848));
#12228=CARTESIAN_POINT('Ctrl Pts',(3.5000008470667,-1.33997810357527,0.628091493562486));
#12229=CARTESIAN_POINT('Ctrl Pts',(3.50000049017339,-1.34160279315579,0.620357239364781));
#12230=CARTESIAN_POINT('Ctrl Pts',(3.50000026118253,-1.3426452308862,0.615394766232079));
#12231=CARTESIAN_POINT('Ctrl Pts',(3.5,-1.34331313055125,0.610351689051435));
#12232=CARTESIAN_POINT('Ctrl Pts',(3.5,-1.34358136363184,0.605270327458634));
#12233=CARTESIAN_POINT('',(3.5,0.723888888888889,0.7));
#12234=CARTESIAN_POINT('Ctrl Pts',(3.5,1.37552980833516,0.));
#12235=CARTESIAN_POINT('Ctrl Pts',(3.5,1.37020035376703,0.10097504527886));
#12236=CARTESIAN_POINT('Ctrl Pts',(3.5,1.36487063968137,0.201951358354439));
#12237=CARTESIAN_POINT('Ctrl Pts',(3.5,1.35422120417274,0.403707279015233));
#12238=CARTESIAN_POINT('Ctrl Pts',(3.5,1.34890134846466,0.504489444860456));
#12239=CARTESIAN_POINT('Ctrl Pts',(3.5,1.34358136363184,0.605270327458635));
#12240=CARTESIAN_POINT('Ctrl Pts',(3.50000000097418,-1.37552980835478,3.46944695195361E-18));
#12241=CARTESIAN_POINT('Ctrl Pts',(3.50374047168104,-1.36494504174376,0.201972406882836));
#12242=CARTESIAN_POINT('Ctrl Pts',(3.50748098869546,-1.35436027657305,0.403944812985359));
#12243=CARTESIAN_POINT('Ctrl Pts',(3.51122155284351,-1.34377551287676,0.605917218294091));
#12244=CARTESIAN_POINT('Ctrl Pts',(2.69119625874569,-1.35924722858667,-7.54309614812119E-5));
#12245=CARTESIAN_POINT('Ctrl Pts',(2.69653217397324,-1.34866266892899,0.20189683354744));
#12246=CARTESIAN_POINT('Ctrl Pts',(2.70186816749714,-1.3380781117335,0.403869096002786));
#12247=CARTESIAN_POINT('Ctrl Pts',(2.7072042346663,-1.32749355863083,0.605841357314298));
#12248=CARTESIAN_POINT('Ctrl Pts',(1.88267190563219,-1.32763345268679,-0.000212792412547521));
#12249=CARTESIAN_POINT('Ctrl Pts',(1.88960380459144,-1.31704931403188,0.201759213581099));
#12250=CARTESIAN_POINT('Ctrl Pts',(1.89653581411498,-1.30646518166523,0.403731216009517));
#12251=CARTESIAN_POINT('Ctrl Pts',(1.90346792975642,-1.29588105699583,0.605703215867581));
#12252=CARTESIAN_POINT('Ctrl Pts',(1.07441451989529,-1.27728918272486,-0.000429194541766893));
#12253=CARTESIAN_POINT('Ctrl Pts',(1.08294287068452,-1.26670581246828,0.201542410257184));
#12254=CARTESIAN_POINT('Ctrl Pts',(1.09147136321593,-1.25612245578053,0.403514009799157));
#12255=CARTESIAN_POINT('Ctrl Pts',(1.09999999999989,-1.24553911298205,0.605485603995245));
#12256=CARTESIAN_POINT('Ctrl Pts',(1.09999999916631,-1.24553911263844,0.605485603997431));
#12257=CARTESIAN_POINT('Ctrl Pts',(1.89930203168262,-1.29563783986497,0.605377360150118));
#12258=CARTESIAN_POINT('Ctrl Pts',(2.69958486793449,-1.32722445934619,0.605308375488923));
#12259=CARTESIAN_POINT('Ctrl Pts',(3.5,-1.34358136363184,0.605270327458634));
#12260=CARTESIAN_POINT('Ctrl Pts',(3.50204003610941,-1.24374118183538,0.7));
#12261=CARTESIAN_POINT('Ctrl Pts',(2.70080437300401,-1.2273695200909,0.7));
#12262=CARTESIAN_POINT('Ctrl Pts',(1.89984199608574,-1.1957170361627,0.7));
#12263=CARTESIAN_POINT('Ctrl Pts',(1.1,-1.14549341399196,0.7));
#12264=CARTESIAN_POINT('Ctrl Pts',(3.50144932661635,-1.27265074030048,0.7));
#12265=CARTESIAN_POINT('Ctrl Pts',(2.6998452019678,-1.25626413437997,0.699999727319846));
#12266=CARTESIAN_POINT('Ctrl Pts',(1.89847848223078,-1.22458382597074,0.70000077422621));
#12267=CARTESIAN_POINT('Ctrl Pts',(1.09819048660397,-1.17431102498992,0.7));
#12268=CARTESIAN_POINT('Ctrl Pts',(3.50042536655637,-1.322763754511,0.676632802377821));
#12269=CARTESIAN_POINT('Ctrl Pts',(2.69818680938114,-1.3063522351595,0.67664530655333));
#12270=CARTESIAN_POINT('Ctrl Pts',(1.89610976425884,-1.27462253270773,0.67666760713801));
#12271=CARTESIAN_POINT('Ctrl Pts',(1.09505363188407,-1.22426736091617,0.676703190608825));
#12272=CARTESIAN_POINT('Ctrl Pts',(3.50002334924346,-1.34243864233338,0.626926882269943));
#12273=CARTESIAN_POINT('Ctrl Pts',(2.6975332861013,-1.32603127467068,0.626959208652505));
#12274=CARTESIAN_POINT('Ctrl Pts',(1.89518106151152,-1.29430885982199,0.62701751976321));
#12275=CARTESIAN_POINT('Ctrl Pts',(1.09381704710221,-1.24396073223232,0.627109609335854));
#12276=CARTESIAN_POINT('Ctrl Pts',(3.5,-1.34358136363184,0.605270327458634));
#12277=CARTESIAN_POINT('Ctrl Pts',(2.69749615303,-1.32718177535833,0.605308474776761));
#12278=CARTESIAN_POINT('Ctrl Pts',(1.89512529323683,-1.29547288309274,0.605377720397184));
#12279=CARTESIAN_POINT('Ctrl Pts',(1.09374258853658,-1.24514653057163,0.605486452199395));
#12280=CARTESIAN_POINT('Ctrl Pts',(3.49999999991875,-1.24369946470729,0.7));
#12281=CARTESIAN_POINT('Ctrl Pts',(3.26917843083003,-1.23897560807887,0.7));
#12282=CARTESIAN_POINT('Ctrl Pts',(3.03837960179139,-1.23298334389983,0.7));
#12283=CARTESIAN_POINT('Ctrl Pts',(2.80762376541487,-1.22564400623233,0.7));
#12284=CARTESIAN_POINT('Ctrl Pts',(2.57739190516312,-1.2178709162388,0.7));
#12285=CARTESIAN_POINT('Ctrl Pts',(2.08463535466707,-1.20026407570248,0.7));
#12286=CARTESIAN_POINT('Ctrl Pts',(1.59210562457525,-1.17639367564078,0.7));
#12287=CARTESIAN_POINT('Ctrl Pts',(1.1,-1.14549341399196,0.7));
#12288=CARTESIAN_POINT('Origin',(5.4,-8.11656130105013E-18,0.7));
#12289=CARTESIAN_POINT('Ctrl Pts',(1.0744145198953,1.27728918272486,-0.000429194541767127));
#12290=CARTESIAN_POINT('Ctrl Pts',(1.08294287068452,1.26670581246828,0.201542410257184));
#12291=CARTESIAN_POINT('Ctrl Pts',(1.09147136321593,1.25612245578053,0.403514009799157));
#12292=CARTESIAN_POINT('Ctrl Pts',(1.0999999999999,1.24553911298205,0.605485603995245));
#12293=CARTESIAN_POINT('Ctrl Pts',(1.88267190563235,1.3276334526868,-0.000212792412547728));
#12294=CARTESIAN_POINT('Ctrl Pts',(1.8896038045916,1.31704931403189,0.201759213581098));
#12295=CARTESIAN_POINT('Ctrl Pts',(1.89653581411514,1.30646518166524,0.403731216009517));
#12296=CARTESIAN_POINT('Ctrl Pts',(1.90346792975658,1.29588105699584,0.605703215867581));
#12297=CARTESIAN_POINT('Ctrl Pts',(2.69119625874601,1.35924722858668,-7.54309614812134E-5));
#12298=CARTESIAN_POINT('Ctrl Pts',(2.69653217397356,1.348662668929,0.201896833547441));
#12299=CARTESIAN_POINT('Ctrl Pts',(2.70186816749745,1.33807811173351,0.403869096002786));
#12300=CARTESIAN_POINT('Ctrl Pts',(2.70720423466661,1.32749355863085,0.605841357314298));
#12301=CARTESIAN_POINT('Ctrl Pts',(3.50000000097466,1.37552980835479,-3.81639164714898E-17));
#12302=CARTESIAN_POINT('Ctrl Pts',(3.50374047168151,1.36494504174377,0.201972406882836));
#12303=CARTESIAN_POINT('Ctrl Pts',(3.50748098869594,1.35436027657306,0.403944812985359));
#12304=CARTESIAN_POINT('Ctrl Pts',(3.51122155284398,1.34377551287677,0.605917218294091));
#12305=CARTESIAN_POINT('Origin',(0.9,1.34328341716202,0.));
#12306=CARTESIAN_POINT('',(0.9,-1.23261418131727,0.605513513251856));
#12307=CARTESIAN_POINT('Ctrl Pts',(0.9,-1.23261418131727,0.605513513251856));
#12308=CARTESIAN_POINT('Ctrl Pts',(0.9,-1.23820195798151,0.504544236118289));
#12309=CARTESIAN_POINT('Ctrl Pts',(0.9,-1.24378834611607,0.403573587101897));
#12310=CARTESIAN_POINT('Ctrl Pts',(0.9,-1.25495246062481,0.201736610752668));
#12311=CARTESIAN_POINT('Ctrl Pts',(0.9,-1.26053033259331,0.100867703930409));
#12312=CARTESIAN_POINT('Ctrl Pts',(0.9,-1.266106713614,0.));
#12313=CARTESIAN_POINT('',(0.9,-1.13254484134404,0.7));
#12314=CARTESIAN_POINT('Ctrl Pts',(0.899999999937205,-1.13254484130906,
0.7));
#12315=CARTESIAN_POINT('Ctrl Pts',(0.899999996287105,-1.14047016437301,
0.699999998205918));
#12316=CARTESIAN_POINT('Ctrl Pts',(0.900001280561548,-1.14833327216777,
0.699006663725481));
#12317=CARTESIAN_POINT('Ctrl Pts',(0.900002371513522,-1.15599299513142,
0.697119896446058));
#12318=CARTESIAN_POINT('Ctrl Pts',(0.900002982478546,-1.16028266409831,
0.696063251566776));
#12319=CARTESIAN_POINT('Ctrl Pts',(0.900003528700818,-1.16450859688491,
0.694725368779139));
#12320=CARTESIAN_POINT('Ctrl Pts',(0.900003857331964,-1.16864431737637,
0.693116947675672));
#12321=CARTESIAN_POINT('Ctrl Pts',(0.900004447924614,-1.17607674172948,
0.690226407030055));
#12322=CARTESIAN_POINT('Ctrl Pts',(0.900004211500339,-1.18313828052408,
0.686496282267003));
#12323=CARTESIAN_POINT('Ctrl Pts',(0.900003280035406,-1.18968205680082,
0.682006679400108));
#12324=CARTESIAN_POINT('Ctrl Pts',(0.900002768383153,-1.19327654302499,
0.679540547464272));
#12325=CARTESIAN_POINT('Ctrl Pts',(0.900002064672634,-1.19671453445753,
0.676844382327844));
#12326=CARTESIAN_POINT('Ctrl Pts',(0.900001450170085,-1.19996775918788,
0.673925988054463));
#12327=CARTESIAN_POINT('Ctrl Pts',(0.900000850201302,-1.20314404102283,
0.67107661751105));
#12328=CARTESIAN_POINT('Ctrl Pts',(0.900000329673364,-1.20612495630093,
0.668032594545539));
#12329=CARTESIAN_POINT('Ctrl Pts',(0.900000346081477,-1.20888784276431,
0.664805176146368));
#12330=CARTESIAN_POINT('Ctrl Pts',(0.900000376514472,-1.21401231436848,
0.658819112599938));
#12331=CARTESIAN_POINT('Ctrl Pts',(0.900002057232535,-1.21838968018573,
0.652203523053766));
#12332=CARTESIAN_POINT('Ctrl Pts',(0.900002698394847,-1.22195969054856,
0.645123732731769));
#12333=CARTESIAN_POINT('Ctrl Pts',(0.900002763240662,-1.22232075393107,
0.644407697543824));
#12334=CARTESIAN_POINT('Ctrl Pts',(0.90000282009371,-1.22267351953901,0.643686895083047));
#12335=CARTESIAN_POINT('Ctrl Pts',(0.900002868017411,-1.22301789747605,
0.642961485862499));
#12336=CARTESIAN_POINT('Ctrl Pts',(0.900003341628975,-1.22642125256928,
0.635792544708285));
#12337=CARTESIAN_POINT('Ctrl Pts',(0.900002645022176,-1.22896979279554,
0.628258742918086));
#12338=CARTESIAN_POINT('Ctrl Pts',(0.900001532827652,-1.23061007098772,
0.6205286650049));
#12339=CARTESIAN_POINT('Ctrl Pts',(0.900000822323555,-1.23165793118585,
0.61559045329652));
#12340=CARTESIAN_POINT('Ctrl Pts',(0.900000000000001,-1.23233426661673,
0.610571479357261));
#12341=CARTESIAN_POINT('Ctrl Pts',(0.900000000000001,-1.23261418131727,
0.605513513251856));
#12342=CARTESIAN_POINT('',(0.9,1.13254484134404,0.7));
#12343=CARTESIAN_POINT('',(0.9,0.671641708581009,0.7));
#12344=CARTESIAN_POINT('',(0.9,1.23261418131727,0.605513513251856));
#12345=CARTESIAN_POINT('Ctrl Pts',(0.9,1.23261418131727,0.605513513251856));
#12346=CARTESIAN_POINT('Ctrl Pts',(0.9,1.23217633603244,0.613425232807268));
#12347=CARTESIAN_POINT('Ctrl Pts',(0.900001832787994,1.23077105609892,0.621244170085157));
#12348=CARTESIAN_POINT('Ctrl Pts',(0.900002580745575,1.22848219166492,0.628809599741497));
#12349=CARTESIAN_POINT('Ctrl Pts',(0.900002993068559,1.22722042035689,0.632980157827643));
#12350=CARTESIAN_POINT('Ctrl Pts',(0.90000314174678,1.22568915198244,0.637073706995481));
#12351=CARTESIAN_POINT('Ctrl Pts',(0.900002971484041,1.2238959908032,0.641061424759933));
#12352=CARTESIAN_POINT('Ctrl Pts',(0.900002662567364,1.22064256379503,0.648296551655426));
#12353=CARTESIAN_POINT('Ctrl Pts',(0.900001146653719,1.21656554418039,0.655104870690721));
#12354=CARTESIAN_POINT('Ctrl Pts',(0.900000540233788,1.21172928299109,0.66132323772617));
#12355=CARTESIAN_POINT('Ctrl Pts',(0.900000424918953,1.21080963534652,0.66250570210793));
#12356=CARTESIAN_POINT('Ctrl Pts',(0.900000351402035,1.20986240082127,0.663666762843393));
#12357=CARTESIAN_POINT('Ctrl Pts',(0.900000346234225,1.20888784277449,0.664805176146358));
#12358=CARTESIAN_POINT('Ctrl Pts',(0.900000336405833,1.20703438079614,0.666970266034709));
#12359=CARTESIAN_POINT('Ctrl Pts',(0.900000571869483,1.20508211779724,0.669053482241208));
#12360=CARTESIAN_POINT('Ctrl Pts',(0.900000903580486,1.20303784749416,0.671051418948595));
#12361=CARTESIAN_POINT('Ctrl Pts',(0.900001825932764,1.19735357006848,0.676606861644505));
#12362=CARTESIAN_POINT('Ctrl Pts',(0.900003332967427,1.19102482074992,0.681443262092019));
#12363=CARTESIAN_POINT('Ctrl Pts',(0.900003895332687,1.18421635668109,0.685507797106414));
#12364=CARTESIAN_POINT('Ctrl Pts',(0.900004254598985,1.17986677848026,0.688104419886002));
#12365=CARTESIAN_POINT('Ctrl Pts',(0.9000042929279,1.17532044218795,0.69038534615497));
#12366=CARTESIAN_POINT('Ctrl Pts',(0.900003997675654,1.17061445353731,0.692327416690341));
#12367=CARTESIAN_POINT('Ctrl Pts',(0.900003537640084,1.16328200409216,0.695353376818313));
#12368=CARTESIAN_POINT('Ctrl Pts',(0.900002259964378,1.15564663185935,0.697524398440697));
#12369=CARTESIAN_POINT('Ctrl Pts',(0.900001215101098,1.14785635641255,0.698771715080855));
#12370=CARTESIAN_POINT('Ctrl Pts',(0.900000537649455,1.14280542295857,0.699580430175527));
#12371=CARTESIAN_POINT('Ctrl Pts',(0.899999997568109,1.13768876957788,0.699999998835552));
#12372=CARTESIAN_POINT('Ctrl Pts',(0.899999999937205,1.13254484130906,0.7));
#12373=CARTESIAN_POINT('Ctrl Pts',(0.9,1.266106713614,0.));
#12374=CARTESIAN_POINT('Ctrl Pts',(0.9,1.26053025554556,0.100869097599589));
#12375=CARTESIAN_POINT('Ctrl Pts',(0.9,1.25495230648558,0.201739398169819));
#12376=CARTESIAN_POINT('Ctrl Pts',(0.9,1.24378819189631,0.403576374532447));
#12377=CARTESIAN_POINT('Ctrl Pts',(0.9,1.23820188085298,0.504545629805417));
#12378=CARTESIAN_POINT('Ctrl Pts',(0.9,1.23261418131727,0.605513513251856));
#12379=CARTESIAN_POINT('Ctrl Pts',(0.900000000000002,-1.266106713614,-8.15320033709099E-17));
#12380=CARTESIAN_POINT('Ctrl Pts',(0.908871090277923,-1.25552568177643,
0.201930159665972));
#12381=CARTESIAN_POINT('Ctrl Pts',(0.917742329685194,-1.24494466498547,
0.403860313587921));
#12382=CARTESIAN_POINT('Ctrl Pts',(0.926613720860141,-1.23436366359623,
0.605790461668883));
#12383=CARTESIAN_POINT('Ctrl Pts',(0.697441255022372,-1.25280938151844,
-5.71013218131409E-5));
#12384=CARTESIAN_POINT('Ctrl Pts',(0.706712389899261,-1.24222855501813,
0.201872952723963));
#12385=CARTESIAN_POINT('Ctrl Pts',(0.71598368260269,-1.23164774534186,0.403803000441224));
#12386=CARTESIAN_POINT('Ctrl Pts',(0.725255135891715,-1.22106695288555,
0.605733041729342));
#12387=CARTESIAN_POINT('Ctrl Pts',(0.494899146035781,-1.23832021354117,
-0.000119230777047918));
#12388=CARTESIAN_POINT('Ctrl Pts',(0.504570354086872,-1.2277396148863,0.201810708652083));
#12389=CARTESIAN_POINT('Ctrl Pts',(0.514241728780064,-1.21715903502506,
0.403740641123913));
#12390=CARTESIAN_POINT('Ctrl Pts',(0.523913273026478,-1.20657847439907,
0.605670566527588));
#12391=CARTESIAN_POINT('Ctrl Pts',(0.292373353339556,-1.22258574808743,
-0.000186633859775947));
#12392=CARTESIAN_POINT('Ctrl Pts',(0.302444661323169,-1.21200540195431,
0.201743181663441));
#12393=CARTESIAN_POINT('Ctrl Pts',(0.312516144861689,-1.20142507679253,
0.403672989556125));
#12394=CARTESIAN_POINT('Ctrl Pts',(0.322587807049886,-1.190844773096,0.605602789690272));
#12395=CARTESIAN_POINT('',(0.32407846024449,-1.19096124572524,0.605603291426262));
#12396=CARTESIAN_POINT('Ctrl Pts',(0.292382661757373,-1.22257596919059,
-1.26634813746307E-16));
#12397=CARTESIAN_POINT('Ctrl Pts',(0.302948004341657,-1.21203750712027,
0.201867748891544));
#12398=CARTESIAN_POINT('Ctrl Pts',(0.313513270922098,-1.20149926476964,
0.403735512620674));
#12399=CARTESIAN_POINT('Ctrl Pts',(0.324078460244491,-1.19096124572524,
0.605603291426262));
#12400=CARTESIAN_POINT('Ctrl Pts',(0.324078460244487,-1.19096124572524,
0.605603291426262));
#12401=CARTESIAN_POINT('Ctrl Pts',(0.515976798438381,-1.20595780001216,
0.605571001180369));
#12402=CARTESIAN_POINT('Ctrl Pts',(0.707956283694857,-1.21982772882273,
0.605541108414459));
#12403=CARTESIAN_POINT('Ctrl Pts',(0.900000000000001,-1.23261418131727,
0.605513513251856));
#12404=CARTESIAN_POINT('Ctrl Pts',(0.906632491847682,-1.13298681949577,
0.7));
#12405=CARTESIAN_POINT('Ctrl Pts',(0.714963137593258,-1.12022681655782,
0.7));
#12406=CARTESIAN_POINT('Ctrl Pts',(0.52336552158394,-1.10638609587519,0.7));
#12407=CARTESIAN_POINT('Ctrl Pts',(0.331856371369197,-1.09142177001972,
0.7));
#12408=CARTESIAN_POINT('Ctrl Pts',(0.904714827274509,-1.16179226195561,
0.7));
#12409=CARTESIAN_POINT('Ctrl Pts',(0.712937153454425,-1.14901967286075,
0.69999980360337));
#12410=CARTESIAN_POINT('Ctrl Pts',(0.521230340369869,-1.13516557394852,
0.700000229443053));
#12411=CARTESIAN_POINT('Ctrl Pts',(0.329608751265076,-1.12018616744754,
0.7));
#12412=CARTESIAN_POINT('Ctrl Pts',(0.901389714107723,-1.21173913866089,
0.676722045797292));
#12413=CARTESIAN_POINT('Ctrl Pts',(0.709425477581998,-1.19894546296063,
0.676731074746188));
#12414=CARTESIAN_POINT('Ctrl Pts',(0.517526696841433,-1.18506766126723,
0.67674067107047));
#12415=CARTESIAN_POINT('Ctrl Pts',(0.325711429829026,-1.17006296935233,
0.676751229163451));
#12416=CARTESIAN_POINT('Ctrl Pts',(0.900079298017777,-1.23142303740181,
0.627132481749528));
#12417=CARTESIAN_POINT('Ctrl Pts',(0.708040181852795,-1.21863106773591,
0.627155851652593));
#12418=CARTESIAN_POINT('Ctrl Pts',(0.516066269599777,-1.20475540724405,
0.627181012790208));
#12419=CARTESIAN_POINT('Ctrl Pts',(0.324172915772929,-1.18975243096407,
0.627208352638976));
#12420=CARTESIAN_POINT('Ctrl Pts',(0.900000000000001,-1.23261418131727,
0.605513513251856));
#12421=CARTESIAN_POINT('Ctrl Pts',(0.707956283694857,-1.21982772882273,
0.605541108414459));
#12422=CARTESIAN_POINT('Ctrl Pts',(0.515976798438381,-1.20595780001216,
0.605571001180369));
#12423=CARTESIAN_POINT('Ctrl Pts',(0.324078460244487,-1.19096124572524,
0.605603291426262));
#12424=CARTESIAN_POINT('',(0.3318563713692,-1.09142177001972,0.7));
#12425=CARTESIAN_POINT('Origin',(0.3318563713692,-1.09142177001972,0.6));
#12426=CARTESIAN_POINT('Ctrl Pts',(0.899999999937167,-1.13254484130906,
0.7));
#12427=CARTESIAN_POINT('Ctrl Pts',(0.710543123935439,-1.11990737114256,
0.7));
#12428=CARTESIAN_POINT('Ctrl Pts',(0.521156529292483,-1.10621348751457,
0.7));
#12429=CARTESIAN_POINT('Ctrl Pts',(0.331856371369197,-1.09142177001972,
0.7));
#12430=CARTESIAN_POINT('Origin',(5.4,-8.11656130105013E-18,0.7));
#12431=CARTESIAN_POINT('',(0.3318563713692,1.09142177001972,0.7));
#12432=CARTESIAN_POINT('',(0.3318563713692,-0.7,0.7));
#12433=CARTESIAN_POINT('Ctrl Pts',(0.3318563713692,1.09142177001972,0.7));
#12434=CARTESIAN_POINT('Ctrl Pts',(0.521156529292483,1.10621348751457,0.7));
#12435=CARTESIAN_POINT('Ctrl Pts',(0.710543123935438,1.11990737114256,0.7));
#12436=CARTESIAN_POINT('Ctrl Pts',(0.899999999937165,1.13254484130906,0.7));
#12437=CARTESIAN_POINT('Ctrl Pts',(0.292373353339556,1.22258574808743,-0.000186633859776018));
#12438=CARTESIAN_POINT('Ctrl Pts',(0.30244466132317,1.21200540195431,0.20174318166344));
#12439=CARTESIAN_POINT('Ctrl Pts',(0.31251614486169,1.20142507679253,0.403672989556124));
#12440=CARTESIAN_POINT('Ctrl Pts',(0.322587807049886,1.190844773096,0.605602789690271));
#12441=CARTESIAN_POINT('Ctrl Pts',(0.494899146035781,1.23832021354117,-0.000119230777047989));
#12442=CARTESIAN_POINT('Ctrl Pts',(0.504570354086872,1.2277396148863,0.201810708652083));
#12443=CARTESIAN_POINT('Ctrl Pts',(0.514241728780064,1.21715903502506,0.403740641123914));
#12444=CARTESIAN_POINT('Ctrl Pts',(0.523913273026478,1.20657847439907,0.605670566527587));
#12445=CARTESIAN_POINT('Ctrl Pts',(0.697441255022371,1.25280938151844,-5.71013218130602E-5));
#12446=CARTESIAN_POINT('Ctrl Pts',(0.70671238989926,1.24222855501813,0.201872952723963));
#12447=CARTESIAN_POINT('Ctrl Pts',(0.715983682602689,1.23164774534186,0.403803000441224));
#12448=CARTESIAN_POINT('Ctrl Pts',(0.725255135891714,1.22106695288555,0.605733041729342));
#12449=CARTESIAN_POINT('Ctrl Pts',(0.9,1.266106713614,1.73472347597681E-18));
#12450=CARTESIAN_POINT('Ctrl Pts',(0.908871090277921,1.25552568177643,0.201930159665973));
#12451=CARTESIAN_POINT('Ctrl Pts',(0.917742329685192,1.24494466498547,0.403860313587921));
#12452=CARTESIAN_POINT('Ctrl Pts',(0.92661372086014,1.23436366359623,0.605790461668883));
#12453=CARTESIAN_POINT('',(0.32407846024449,1.19096124572524,0.605603291426262));
#12454=CARTESIAN_POINT('Ctrl Pts',(0.9,1.23261418131727,0.605513513251856));
#12455=CARTESIAN_POINT('Ctrl Pts',(0.707956283694857,1.21982772882273,0.605541108414459));
#12456=CARTESIAN_POINT('Ctrl Pts',(0.515976798438382,1.20595780001216,0.60557100118037));
#12457=CARTESIAN_POINT('Ctrl Pts',(0.32407846024449,1.19096124572524,0.605603291426262));
#12458=CARTESIAN_POINT('Ctrl Pts',(0.324078460244491,1.19096124572524,0.605603291426262));
#12459=CARTESIAN_POINT('Ctrl Pts',(0.313513270922098,1.20149926476964,0.403735512620674));
#12460=CARTESIAN_POINT('Ctrl Pts',(0.302948004341658,1.21203750712026,0.201867748891544));
#12461=CARTESIAN_POINT('Ctrl Pts',(0.292382661757373,1.22257596919059,3.4477629085039E-17));
#12462=CARTESIAN_POINT('Ctrl Pts',(0.3318563713692,1.09142177001972,0.7));
#12463=CARTESIAN_POINT('Ctrl Pts',(0.523365521583941,1.10638609587519,0.7));
#12464=CARTESIAN_POINT('Ctrl Pts',(0.714963137593258,1.12022681655782,0.7));
#12465=CARTESIAN_POINT('Ctrl Pts',(0.906632491847681,1.13298681949577,0.7));
#12466=CARTESIAN_POINT('Ctrl Pts',(0.329608751265078,1.12018616744754,0.7));
#12467=CARTESIAN_POINT('Ctrl Pts',(0.52123034036987,1.13516557394852,0.700000229443053));
#12468=CARTESIAN_POINT('Ctrl Pts',(0.712937153454426,1.14901967286075,0.699999803603371));
#12469=CARTESIAN_POINT('Ctrl Pts',(0.904714827274509,1.16179226195561,0.700000000000001));
#12470=CARTESIAN_POINT('Ctrl Pts',(0.325711429829028,1.17006296935233,0.676751229163452));
#12471=CARTESIAN_POINT('Ctrl Pts',(0.517526696841433,1.18506766126723,0.67674067107047));
#12472=CARTESIAN_POINT('Ctrl Pts',(0.709425477581997,1.19894546296063,0.676731074746189));
#12473=CARTESIAN_POINT('Ctrl Pts',(0.901389714107722,1.21173913866089,0.676722045797292));
#12474=CARTESIAN_POINT('Ctrl Pts',(0.324172915772932,1.18975243096407,0.627208352638976));
#12475=CARTESIAN_POINT('Ctrl Pts',(0.516066269599778,1.20475540724405,0.627181012790208));
#12476=CARTESIAN_POINT('Ctrl Pts',(0.708040181852794,1.21863106773591,0.627155851652593));
#12477=CARTESIAN_POINT('Ctrl Pts',(0.900079298017776,1.23142303740181,0.627132481749528));
#12478=CARTESIAN_POINT('Ctrl Pts',(0.32407846024449,1.19096124572524,0.605603291426262));
#12479=CARTESIAN_POINT('Ctrl Pts',(0.515976798438382,1.20595780001216,0.60557100118037));
#12480=CARTESIAN_POINT('Ctrl Pts',(0.707956283694857,1.21982772882273,0.605541108414459));
#12481=CARTESIAN_POINT('Ctrl Pts',(0.9,1.23261418131727,0.605513513251856));
#12482=CARTESIAN_POINT('Origin',(0.331856371369202,1.09142177001972,0.6));
#12483=CARTESIAN_POINT('Origin',(0.331856371369202,1.09142177001972,0.6));
#12484=CARTESIAN_POINT('Origin',(0.331856371369201,1.09142177001972,0.6));
#12485=CARTESIAN_POINT('Origin',(0.331856371369202,1.09142177001972,0.6));
#12486=CARTESIAN_POINT('Origin',(10.4681436286308,1.08420482079361,0.6));
#12487=CARTESIAN_POINT('Origin',(10.4681436276939,1.08420482084454,0.6));
#12488=CARTESIAN_POINT('',(10.5680065821063,1.08420482079361,0.605233595624295));
#12489=CARTESIAN_POINT('Origin',(10.4681436286308,1.08420482079361,0.6));
#12490=CARTESIAN_POINT('Origin',(10.4681436286308,1.08420482079361,0.6));
#12491=CARTESIAN_POINT('Origin',(0.3318563713692,-1.09142177001972,0.6));
#12492=CARTESIAN_POINT('Origin',(0.331856371369201,-1.09142177001972,0.6));
#12493=CARTESIAN_POINT('Origin',(0.3318563713692,-1.09142177001972,0.6));
#12494=CARTESIAN_POINT('Origin',(0.3318563713692,-0.7,0.6));
#12495=CARTESIAN_POINT('Ctrl Pts',(0.2922895713475,-1.22266882276207,-0.00177864096060679));
#12496=CARTESIAN_POINT('Ctrl Pts',(0.302885944515497,-1.21209940820877,
0.200681988163859));
#12497=CARTESIAN_POINT('Ctrl Pts',(0.313482241236256,-1.20153021465708,
0.403142632212487));
#12498=CARTESIAN_POINT('Ctrl Pts',(0.324078460244491,-1.19096124572524,
0.605603291426262));
#12499=CARTESIAN_POINT('Ctrl Pts',(0.264022491930188,-1.22039553779506,
-0.000415890128406236));
#12500=CARTESIAN_POINT('Ctrl Pts',(0.274621881512248,-1.20982222712748,
0.202044379074236));
#12501=CARTESIAN_POINT('Ctrl Pts',(0.285221154833576,-1.19924944554801,
0.404504681968985));
#12502=CARTESIAN_POINT('Ctrl Pts',(0.29582042516239,-1.18867654001483,0.606964977361795));
#12503=CARTESIAN_POINT('Ctrl Pts',(0.216712469170969,-1.1940874043406,0.000690255297866666));
#12504=CARTESIAN_POINT('Ctrl Pts',(0.227319688237882,-1.18351239299796,
0.203150045648192));
#12505=CARTESIAN_POINT('Ctrl Pts',(0.237926932441998,-1.17293746916702,
0.405609838636422));
#12506=CARTESIAN_POINT('Ctrl Pts',(0.248534117816369,-1.1623628476683,0.608069650238703));
#12507=CARTESIAN_POINT('Ctrl Pts',(0.200219987929043,-1.14439035743082,
-0.00103956457010847));
#12508=CARTESIAN_POINT('Ctrl Pts',(0.210830491339948,-1.13382006821851,
0.201420337884579));
#12509=CARTESIAN_POINT('Ctrl Pts',(0.221440906577676,-1.12324995278282,
0.403880253819325));
#12510=CARTESIAN_POINT('Ctrl Pts',(0.232051411471599,-1.11268010558856,
0.606340179010355));
#12511=CARTESIAN_POINT('Ctrl Pts',(0.200161975173303,-1.12312592850316,
-0.00214651389202307));
#12512=CARTESIAN_POINT('Ctrl Pts',(0.210772455448684,-1.11255764422181,
0.200313510564959));
#12513=CARTESIAN_POINT('Ctrl Pts',(0.221382936352032,-1.1019895901204,0.402773547004277));
#12514=CARTESIAN_POINT('Ctrl Pts',(0.231993417893744,-1.09142177001972,
0.605233595624295));
#12515=CARTESIAN_POINT('Origin',(10.4681436286308,-1.08420482109828,0.6));
#12516=CARTESIAN_POINT('',(10.5680065821063,-1.08420482079361,0.605233595624295));
#12517=CARTESIAN_POINT('Origin',(10.4681436286308,-1.08420482099672,0.600000000000001));
#12518=CARTESIAN_POINT('Origin',(10.4681436286308,-1.08420482109828,0.6));
#12519=CARTESIAN_POINT('Origin',(10.4681436286308,0.7,0.6));
#12520=CARTESIAN_POINT('',(10.5680065821063,0.7,0.605233595624295));
#12521=CARTESIAN_POINT('Ctrl Pts',(10.599839982685,-1.11594741464673,-0.00218387205330164));
#12522=CARTESIAN_POINT('Ctrl Pts',(10.5892288496247,-1.10536637943871,0.200288608282177));
#12523=CARTESIAN_POINT('Ctrl Pts',(10.5786177161011,-1.0947855138519,0.402761097457634));
#12524=CARTESIAN_POINT('Ctrl Pts',(10.5680065821063,-1.08420482079362,0.605233595624295));
#12525=CARTESIAN_POINT('Ctrl Pts',(10.5997613205547,-1.14474784499259,-0.000682909193257743));
#12526=CARTESIAN_POINT('Ctrl Pts',(10.5891501209488,-1.13416481604349,0.201789447273867));
#12527=CARTESIAN_POINT('Ctrl Pts',(10.5785391399155,-1.12358205581644,0.404261829287571));
#12528=CARTESIAN_POINT('Ctrl Pts',(10.5679279386544,-1.11299934606825,0.606734202078189));
#12529=CARTESIAN_POINT('Ctrl Pts',(10.5764119435127,-1.19466846760808,0.000702210001053139));
#12530=CARTESIAN_POINT('Ctrl Pts',(10.5658041809617,-1.18408222297768,0.203174550667819));
#12531=CARTESIAN_POINT('Ctrl Pts',(10.5551963844732,-1.17349608774572,0.405646894856767));
#12532=CARTESIAN_POINT('Ctrl Pts',(10.544588659013,-1.16291012508165,0.608119251464957));
#12533=CARTESIAN_POINT('Ctrl Pts',(10.5269342003857,-1.21442651155969,-0.000858270497959616));
#12534=CARTESIAN_POINT('Ctrl Pts',(10.5163317654776,-1.20384274018949,0.201614467507756));
#12535=CARTESIAN_POINT('Ctrl Pts',(10.5057293269973,-1.1932591813998,0.404087216090532));
#12536=CARTESIAN_POINT('Ctrl Pts',(10.4951269905998,-1.18267571840064,0.606559974437339));
#12537=CARTESIAN_POINT('Ctrl Pts',(10.5053655128635,-1.21565094114741,-0.0019246498908503));
#12538=CARTESIAN_POINT('Ctrl Pts',(10.4947646468921,-1.20506932615592,0.200548282383137));
#12539=CARTESIAN_POINT('Ctrl Pts',(10.4841638390504,-1.19448787589602,0.403021225840181));
#12540=CARTESIAN_POINT('Ctrl Pts',(10.4735630903435,-1.18390659316268,0.605494180667945));
#12541=CARTESIAN_POINT('Ctrl Pts',(10.5997255308004,-1.11583328740478,1.02782365951626E-16));
#12542=CARTESIAN_POINT('Ctrl Pts',(10.589152548365,-1.10529029582828,0.201744523047832));
#12543=CARTESIAN_POINT('Ctrl Pts',(10.5785795654695,-1.09474747266587,0.40348905487273));
#12544=CARTESIAN_POINT('Ctrl Pts',(10.5680065821063,-1.08420482079362,0.605233595624295));
#12545=CARTESIAN_POINT('Ctrl Pts',(10.5053638082297,1.21564923960921,-0.0018920919656423));
#12546=CARTESIAN_POINT('Ctrl Pts',(10.4947635104759,1.20506819181477,0.200569987667808));
#12547=CARTESIAN_POINT('Ctrl Pts',(10.4841632708454,1.19448730873444,0.403032078483127));
#12548=CARTESIAN_POINT('Ctrl Pts',(10.4735630903435,1.18390659316268,0.605494180667945));
#12549=CARTESIAN_POINT('Ctrl Pts',(10.5341220579192,1.21401666636749,-0.000470252816738081));
#12550=CARTESIAN_POINT('Ctrl Pts',(10.5235196325477,1.20343268662274,0.201991562854702));
#12551=CARTESIAN_POINT('Ctrl Pts',(10.5129172908767,1.19284910679518,0.404453403808947));
#12552=CARTESIAN_POINT('Ctrl Pts',(10.5023149573519,1.18226542681329,0.606915239027137));
#12553=CARTESIAN_POINT('Ctrl Pts',(10.5827170203615,1.18801090922716,0.000717463067903341));
#12554=CARTESIAN_POINT('Ctrl Pts',(10.5721088691741,1.17742555398174,0.203178921531494));
#12555=CARTESIAN_POINT('Ctrl Pts',(10.5615007184277,1.16684027916303,0.405640383775807));
#12556=CARTESIAN_POINT('Ctrl Pts',(10.5508925935528,1.15625520969485,0.60810185787831));
#12557=CARTESIAN_POINT('Ctrl Pts',(10.5997792798033,1.13754603572512,-0.00102559206997387));
#12558=CARTESIAN_POINT('Ctrl Pts',(10.5891686973038,1.12696411138589,0.201435946515793));
#12559=CARTESIAN_POINT('Ctrl Pts',(10.5785581831385,1.11638231376635,0.40389749513889));
#12560=CARTESIAN_POINT('Ctrl Pts',(10.5679475995174,1.10580071474959,0.606359050464716));
#12561=CARTESIAN_POINT('Ctrl Pts',(10.5998382764002,1.11594571320176,-0.00215131420076595));
#12562=CARTESIAN_POINT('Ctrl Pts',(10.5892277121014,1.10536524516024,0.200310313518148));
#12563=CARTESIAN_POINT('Ctrl Pts',(10.5786171473394,1.09478494672192,0.402771950076102));
#12564=CARTESIAN_POINT('Ctrl Pts',(10.5680065821063,1.08420482079361,0.605233595624295));
#12565=CARTESIAN_POINT('Ctrl Pts',(10.5680065821063,1.08420482079361,0.605233595624295));
#12566=CARTESIAN_POINT('Ctrl Pts',(10.5785795654695,1.09474747266587,0.40348905487273));
#12567=CARTESIAN_POINT('Ctrl Pts',(10.589152548365,1.10529029582828,0.201744523047831));
#12568=CARTESIAN_POINT('Ctrl Pts',(10.5997255308004,1.11583328740478,1.07661275727811E-16));
#12569=CARTESIAN_POINT('Ctrl Pts',(10.1947388861048,1.09885088260187,0.7));
#12570=CARTESIAN_POINT('Ctrl Pts',(10.285877616441,1.09404209584202,0.7));
#12571=CARTESIAN_POINT('Ctrl Pts',(10.3770124662346,1.0891584122264,0.7));
#12572=CARTESIAN_POINT('Ctrl Pts',(10.4681436286308,1.08420482079361,0.7));
#12573=CARTESIAN_POINT('Ctrl Pts',(10.196260416419,1.12768774893097,0.700000000000001));
#12574=CARTESIAN_POINT('Ctrl Pts',(10.2874149314686,1.12287675076168,0.699999949550842));
#12575=CARTESIAN_POINT('Ctrl Pts',(10.3785648662465,1.11799094453753,0.700000051218742));
#12576=CARTESIAN_POINT('Ctrl Pts',(10.4697107510168,1.11303515260326,0.7));
#12577=CARTESIAN_POINT('Ctrl Pts',(10.1988975981852,1.17766904563614,0.67669140632491));
#12578=CARTESIAN_POINT('Ctrl Pts',(10.2900793016129,1.17285439035486,0.676693724638983));
#12579=CARTESIAN_POINT('Ctrl Pts',(10.3812557252598,1.16796482352885,0.676696026813929));
#12580=CARTESIAN_POINT('Ctrl Pts',(10.4724269697127,1.16300539549315,0.676698381019544));
#12581=CARTESIAN_POINT('Ctrl Pts',(10.1999375452555,1.19737868557977,0.627098033786781));
#12582=CARTESIAN_POINT('Ctrl Pts',(10.2911301919381,1.19256517083271,0.627104033151799));
#12583=CARTESIAN_POINT('Ctrl Pts',(10.382317043787,1.18767684023183,0.627110048826767));
#12584=CARTESIAN_POINT('Ctrl Pts',(10.4734985149421,1.18271860027509,0.627116141711795));
#12585=CARTESIAN_POINT('Ctrl Pts',(10.1999999975038,1.19856231440453,0.605472757505366));
#12586=CARTESIAN_POINT('Ctrl Pts',(10.2911933328565,1.19375025772558,0.605479840815741));
#12587=CARTESIAN_POINT('Ctrl Pts',(10.3823809652617,1.18886335120032,0.605486986548286));
#12588=CARTESIAN_POINT('Ctrl Pts',(10.4735630903435,1.18390659316268,0.605494180667944));
#12589=CARTESIAN_POINT('Ctrl Pts',(0.200159601751749,1.12312829248604,-0.00219180147311912));
#12590=CARTESIAN_POINT('Ctrl Pts',(0.210770873167554,1.11255922017607,0.200283318842441));
#12591=CARTESIAN_POINT('Ctrl Pts',(0.221382145211419,1.10199037808008,0.402758451142111));
#12592=CARTESIAN_POINT('Ctrl Pts',(0.231993417893744,1.09142177001972,0.605233595624295));
#12593=CARTESIAN_POINT('Ctrl Pts',(0.200236952094631,1.15148086499205,-0.000715869007730825));
#12594=CARTESIAN_POINT('Ctrl Pts',(0.210848310847714,1.14090905181173,0.201759082033021));
#12595=CARTESIAN_POINT('Ctrl Pts',(0.221459381762758,1.13033759660317,0.404234066901971));
#12596=CARTESIAN_POINT('Ctrl Pts',(0.232070742664217,1.11976621744484,0.606709040139042));
#12597=CARTESIAN_POINT('Ctrl Pts',(0.222806696702742,1.20067708175657,0.000669311976984441));
#12598=CARTESIAN_POINT('Ctrl Pts',(0.233413416075889,1.19010082554658,0.203144236955742));
#12599=CARTESIAN_POINT('Ctrl Pts',(0.244020198555212,1.17952469009474,0.405619164345205));
#12600=CARTESIAN_POINT('Ctrl Pts',(0.254626870458834,1.16894881850735,0.608094110943904));
#12601=CARTESIAN_POINT('Ctrl Pts',(0.271086891015657,1.22096622390789,-0.000801865493577694));
#12602=CARTESIAN_POINT('Ctrl Pts',(0.281686280594249,1.21039315447922,0.201673594461172));
#12603=CARTESIAN_POINT('Ctrl Pts',(0.292285672737775,1.1998203699977,0.404149068703718));
#12604=CARTESIAN_POINT('Ctrl Pts',(0.302884933932915,1.18924771644243,0.606624555877912));
#12605=CARTESIAN_POINT('Ctrl Pts',(0.292287201081515,1.22267118699778,-0.00182392867695869));
#12606=CARTESIAN_POINT('Ctrl Pts',(0.302884364349574,1.21210098433295,0.200651796350731));
#12607=CARTESIAN_POINT('Ctrl Pts',(0.313481451159089,1.20153100270242,0.403127536304793));
#12608=CARTESIAN_POINT('Ctrl Pts',(0.324078460244491,1.19096124572524,0.605603291426262));
#12609=CARTESIAN_POINT('Origin',(10.6002740930491,1.4,-0.0104671912485891));
#12610=CARTESIAN_POINT('Origin',(0.331856371369202,1.09142177001972,0.6));
#12611=CARTESIAN_POINT('',(0.3318563713692,1.09142177001972,0.9));
#12612=CARTESIAN_POINT('',(0.0322675109428288,1.09142177001972,0.615700786872883));
#12613=CARTESIAN_POINT('Origin',(0.3318563713692,1.09142177001972,0.6));
#12614=CARTESIAN_POINT('',(0.308522637995069,1.39004019713626,0.616809874278785));
#12615=CARTESIAN_POINT('Origin',(0.331856371369202,1.09142177001972,0.6));
#12616=CARTESIAN_POINT('Origin',(0.331856371369201,1.09142177001972,0.6));
#12617=CARTESIAN_POINT('Origin',(10.4681436286308,1.08420482079361,0.6));
#12618=CARTESIAN_POINT('',(10.4681436286308,1.08420482109828,0.9));
#12619=CARTESIAN_POINT('',(10.4844020137689,1.3833101379008,0.616482542003833));
#12620=CARTESIAN_POINT('Origin',(10.4681436258201,1.08420482094639,0.6));
#12621=CARTESIAN_POINT('',(10.7677324890572,1.08420482079361,0.615700786872884));
#12622=CARTESIAN_POINT('Origin',(10.4681436286308,1.08420482079361,0.6));
#12623=CARTESIAN_POINT('Origin',(10.4681436286308,1.08420482079362,0.6));
#12624=CARTESIAN_POINT('Origin',(0.3318563713692,-1.09142177001972,0.6));
#12625=CARTESIAN_POINT('',(0.3318563713692,-1.09142177001972,0.9));
#12626=CARTESIAN_POINT('',(0.308522637995069,-1.39004019713626,0.616809874278785));
#12627=CARTESIAN_POINT('Origin',(0.3318563713692,-1.09142177001972,0.6));
#12628=CARTESIAN_POINT('',(0.0322675109428289,-1.09142177001972,0.615700786872884));
#12629=CARTESIAN_POINT('Origin',(0.3318563713692,-1.09142177001972,0.6));
#12630=CARTESIAN_POINT('Origin',(0.331856371369201,-1.09142177001972,0.6));
#12631=CARTESIAN_POINT('Origin',(0.3318563713692,-0.7,0.6));
#12632=CARTESIAN_POINT('',(0.0322675109428288,-0.7,0.615700786872883));
#12633=CARTESIAN_POINT('',(0.3318563713692,-0.7,0.9));
#12634=CARTESIAN_POINT('Ctrl Pts',(0.276048389810261,-1.42252533450788,
-0.00533608639730399));
#12635=CARTESIAN_POINT('Ctrl Pts',(0.28687338241706,-1.4116967417008,0.202045878554724));
#12636=CARTESIAN_POINT('Ctrl Pts',(0.297698133178874,-1.40086836142621,
0.409427865329919));
#12637=CARTESIAN_POINT('Ctrl Pts',(0.308522637995069,-1.39004019713626,
0.616809874278785));
#12638=CARTESIAN_POINT('Ctrl Pts',(0.191246496057484,-1.41570630783033,
-0.00124775669238285));
#12639=CARTESIAN_POINT('Ctrl Pts',(0.202080757839133,-1.40486573978029,
0.206133102090467));
#12640=CARTESIAN_POINT('Ctrl Pts',(0.212914648880055,-1.39402634701096,
0.413514041581016));
#12641=CARTESIAN_POINT('Ctrl Pts',(0.223748532748767,-1.38318608000504,
0.620894932085382));
#12642=CARTESIAN_POINT('Ctrl Pts',(0.0492682973509243,-1.33685850703924,
0.00207719607616587));
#12643=CARTESIAN_POINT('Ctrl Pts',(0.0601266125734448,-1.32601270457081,
0.209456583216085));
#12644=CARTESIAN_POINT('Ctrl Pts',(0.0709850253737815,-1.3151666447344,
0.416835949794532));
#12645=CARTESIAN_POINT('Ctrl Pts',(0.0818432319483421,-1.30432109509162,
0.624215353109623));
#12646=CARTESIAN_POINT('Ctrl Pts',(-0.000163444061205068,-1.18769013309795,
-0.00311869847265479));
#12647=CARTESIAN_POINT('Ctrl Pts',(0.0107049555364969,-1.17685886333949,
0.204261034729081));
#12648=CARTESIAN_POINT('Ctrl Pts',(0.0215730900970294,-1.16602762920277,
0.411640782964944));
#12649=CARTESIAN_POINT('Ctrl Pts',(0.0324414916763936,-1.15519677672624,
0.619020537031064));
#12650=CARTESIAN_POINT('Ctrl Pts',(-0.00033748371827097,-1.12389640457412,
-0.0064395729582146));
#12651=CARTESIAN_POINT('Ctrl Pts',(0.0105308471731094,-1.11307128361434,
0.200940534347673));
#12652=CARTESIAN_POINT('Ctrl Pts',(0.0213991787230862,-1.10224640406117,
0.408320654220332));
#12653=CARTESIAN_POINT('Ctrl Pts',(0.0322675109428289,-1.09142177001972,
0.615700786872884));
#12654=CARTESIAN_POINT('Ctrl Pts',(0.27632692456468,-1.42224670711126,5.13911829758129E-17));
#12655=CARTESIAN_POINT('Ctrl Pts',(0.287059068122268,-1.41151099373342,
0.20560326985903));
#12656=CARTESIAN_POINT('Ctrl Pts',(0.297790973931072,-1.40077548928706,
0.411206561171438));
#12657=CARTESIAN_POINT('Ctrl Pts',(0.308522637995069,-1.39004019713626,
0.616809874278785));
#12658=CARTESIAN_POINT('Ctrl Pts',(0.0322675109428289,-1.09142177001972,
0.615700786872884));
#12659=CARTESIAN_POINT('Ctrl Pts',(0.0215116733095221,-1.10213436178043,
0.410467178800746));
#12660=CARTESIAN_POINT('Ctrl Pts',(0.0107558363321879,-1.11284719399673,
0.205233583245308));
#12661=CARTESIAN_POINT('Ctrl Pts',(1.76901136968166E-16,-1.12356026268968,
-7.45931094670027E-17));
#12662=CARTESIAN_POINT('Origin',(10.4681436286308,-1.08420482109828,0.6));
#12663=CARTESIAN_POINT('',(10.7677324890572,-1.08420482079361,0.615700786872884));
#12664=CARTESIAN_POINT('',(10.4844020137689,-1.3833101379008,0.616482542003833));
#12665=CARTESIAN_POINT('Origin',(10.4681436286308,-1.08420482079361,0.600000000000001));
#12666=CARTESIAN_POINT('',(10.4681436258201,-1.08420482094639,0.9));
#12667=CARTESIAN_POINT('Origin',(10.4681436286308,-1.08420482109828,0.6));
#12668=CARTESIAN_POINT('Origin',(10.4681436286308,-1.08420482079361,0.6));
#12669=CARTESIAN_POINT('Origin',(10.4681436286308,0.7,0.6));
#12670=CARTESIAN_POINT('',(10.7677324890572,0.7,0.615700786872884));
#12671=CARTESIAN_POINT('',(10.4681436286308,0.7,0.9));
#12672=CARTESIAN_POINT('Ctrl Pts',(10.4681436286308,-1.08420482079361,0.9));
#12673=CARTESIAN_POINT('Ctrl Pts',(9.02115959826777,-1.16285813221549,0.9));
#12674=CARTESIAN_POINT('Ctrl Pts',(5.64262097844114,-1.30550334054488,0.9));
#12675=CARTESIAN_POINT('Ctrl Pts',(2.25816172369615,-1.24194126716656,0.9));
#12676=CARTESIAN_POINT('Ctrl Pts',(0.331856371369198,-1.09142177001972,
0.9));
#12677=CARTESIAN_POINT('Ctrl Pts',(10.4728449957889,-1.17069581622255,0.9));
#12678=CARTESIAN_POINT('Ctrl Pts',(9.02515960257209,-1.24945398332951,0.900002463983243));
#12679=CARTESIAN_POINT('Ctrl Pts',(5.64406008560805,-1.39235654229312,0.899995181674544));
#12680=CARTESIAN_POINT('Ctrl Pts',(2.25481214769604,-1.3286896492945,0.900006992415263));
#12681=CARTESIAN_POINT('Ctrl Pts',(0.325113511056834,-1.17771496230318,
0.9));
#12682=CARTESIAN_POINT('Ctrl Pts',(10.4809942371438,-1.32061731204901,0.830050158657121));
#12683=CARTESIAN_POINT('Ctrl Pts',(9.03210079995546,-1.3995487214628,0.829938185878055));
#12684=CARTESIAN_POINT('Ctrl Pts',(5.64656962219688,-1.54290142969263,0.82970437227026));
#12685=CARTESIAN_POINT('Ctrl Pts',(2.24896854757963,-1.47903552984056,0.829838703712927));
#12686=CARTESIAN_POINT('Ctrl Pts',(0.313425270489114,-1.32729771265557,
0.830156825336737));
#12687=CARTESIAN_POINT('Ctrl Pts',(10.4842082875648,-1.37974615923803,0.681348425135383));
#12688=CARTESIAN_POINT('Ctrl Pts',(9.03482793853036,-1.45862084618981,0.681058092399338));
#12689=CARTESIAN_POINT('Ctrl Pts',(5.64753778607331,-1.60187726023264,0.68045297450285));
#12690=CARTESIAN_POINT('Ctrl Pts',(2.24670449952385,-1.53809938127555,0.680799765935021));
#12691=CARTESIAN_POINT('Ctrl Pts',(0.308806004580392,-1.38641375285276,
0.681625057916928));
#12692=CARTESIAN_POINT('Ctrl Pts',(10.4844020137689,-1.3833101379008,0.616482542003833));
#12693=CARTESIAN_POINT('Ctrl Pts',(9.03499042108131,-1.46211428773623,0.616139856494792));
#12694=CARTESIAN_POINT('Ctrl Pts',(5.64759185703765,-1.60522711936681,0.615422163720642));
#12695=CARTESIAN_POINT('Ctrl Pts',(2.24657199659733,-1.54153220865049,0.615835494619844));
#12696=CARTESIAN_POINT('Ctrl Pts',(0.308522637995066,-1.39004019713626,
0.616809874278785));
#12697=CARTESIAN_POINT('Ctrl Pts',(0.308522637995066,-1.39004019713626,
0.616809874278785));
#12698=CARTESIAN_POINT('Ctrl Pts',(2.24657199659733,-1.54153220865049,0.615835494619844));
#12699=CARTESIAN_POINT('Ctrl Pts',(5.64759185703765,-1.60522711936681,0.615422163720642));
#12700=CARTESIAN_POINT('Ctrl Pts',(9.03499042108131,-1.46211428773623,0.616139856494792));
#12701=CARTESIAN_POINT('Ctrl Pts',(10.4844020137689,-1.3833101379008,0.616482542003833));
#12702=CARTESIAN_POINT('Ctrl Pts',(10.4681436258201,-1.08420482094639,0.900000000000001));
#12703=CARTESIAN_POINT('Ctrl Pts',(9.02115959639274,-1.16285813229465,0.9));
#12704=CARTESIAN_POINT('Ctrl Pts',(5.64262097750198,-1.30550334052724,0.9));
#12705=CARTESIAN_POINT('Ctrl Pts',(2.25816172369615,-1.24194126716656,0.9));
#12706=CARTESIAN_POINT('Ctrl Pts',(0.331856371369198,-1.09142177001972,
0.9));
#12707=CARTESIAN_POINT('Ctrl Pts',(10.8003433549902,-1.11672267507076,-0.00655160349952438));
#12708=CARTESIAN_POINT('Ctrl Pts',(10.7894730668347,-1.10588321133639,0.200865850630566));
#12709=CARTESIAN_POINT('Ctrl Pts',(10.7786027781932,-1.09504392553578,0.408283314033857));
#12710=CARTESIAN_POINT('Ctrl Pts',(10.7677324890572,-1.08420482079361,0.615700786872885));
#12711=CARTESIAN_POINT('Ctrl Pts',(10.8001073672393,-1.20312439623403,-0.00204868896805508));
#12712=CARTESIAN_POINT('Ctrl Pts',(10.7892368724076,-1.19227880391739,0.205368384315645));
#12713=CARTESIAN_POINT('Ctrl Pts',(10.7783670568079,-1.18143370221047,0.41278551899075));
#12714=CARTESIAN_POINT('Ctrl Pts',(10.7674965587017,-1.17058839661753,0.620202606234566));
#12715=CARTESIAN_POINT('Ctrl Pts',(10.7300137544668,-1.35289768637741,0.00210488808650419));
#12716=CARTESIAN_POINT('Ctrl Pts',(10.7191538066016,-1.34204221082848,0.209521911971666));
#12717=CARTESIAN_POINT('Ctrl Pts',(10.7082938463195,-1.33118673671862,0.416938933985702));
#12718=CARTESIAN_POINT('Ctrl Pts',(10.6974340169938,-1.32033143065575,0.624355970618915));
#12719=CARTESIAN_POINT('Ctrl Pts',(10.5816241002662,-1.4121605627967,-0.00257485550010117));
#12720=CARTESIAN_POINT('Ctrl Pts',(10.5707805459565,-1.4013126969686,0.204843391064434));
#12721=CARTESIAN_POINT('Ctrl Pts',(10.5599369567012,-1.39046512672587,0.412261650129749));
#12722=CARTESIAN_POINT('Ctrl Pts',(10.5490937145378,-1.37961751361469,0.619679923312015));
#12723=CARTESIAN_POINT('Ctrl Pts',(10.5169176890673,-1.41583338198674,-0.00577403633861717));
#12724=CARTESIAN_POINT('Ctrl Pts',(10.5060789456421,-1.40499213715574,0.201644806368331));
#12725=CARTESIAN_POINT('Ctrl Pts',(10.4952403861233,-1.39415105487295,0.40906366572247));
#12726=CARTESIAN_POINT('Ctrl Pts',(10.4844020137689,-1.3833101379008,0.616482542003833));
#12727=CARTESIAN_POINT('Ctrl Pts',(10.8,-1.11638029377732,-2.51534904016637E-17));
#12728=CARTESIAN_POINT('Ctrl Pts',(10.7892441634977,-1.10565496086826,0.205233586491178));
#12729=CARTESIAN_POINT('Ctrl Pts',(10.7784883265195,-1.09492980219801,0.410467182062988));
#12730=CARTESIAN_POINT('Ctrl Pts',(10.7677324890572,-1.08420482079361,0.615700786872885));
#12731=CARTESIAN_POINT('Ctrl Pts',(10.4844020137689,-1.3833101379008,0.616482542003833));
#12732=CARTESIAN_POINT('Ctrl Pts',(10.4951398148107,-1.39405045994841,0.410988344812119));
#12733=CARTESIAN_POINT('Ctrl Pts',(10.5058777995597,-1.40479094425298,0.205494164234945));
#12734=CARTESIAN_POINT('Ctrl Pts',(10.5166159648474,-1.4155315881283,-2.5652223401007E-16));
#12735=CARTESIAN_POINT('Ctrl Pts',(10.5169125872774,1.41582827901939,-0.0056764044152427));
#12736=CARTESIAN_POINT('Ctrl Pts',(10.5060755445066,1.40498873522851,0.20170989432247));
#12737=CARTESIAN_POINT('Ctrl Pts',(10.4952386855848,1.39414935393528,0.409096209702196));
#12738=CARTESIAN_POINT('Ctrl Pts',(10.4844020137689,1.3833101379008,0.616482542003833));
#12739=CARTESIAN_POINT('Ctrl Pts',(10.6031877991504,1.41093118264609,-0.00141083033817288));
#12740=CARTESIAN_POINT('Ctrl Pts',(10.5923442181457,1.40008262840665,0.205974657203891));
#12741=CARTESIAN_POINT('Ctrl Pts',(10.5815009048179,1.38923496752292,0.413360205434192));
#12742=CARTESIAN_POINT('Ctrl Pts',(10.5706576147941,1.37838663885266,0.62074571708141));
#12743=CARTESIAN_POINT('Ctrl Pts',(10.7489822201969,1.33286898269122,0.00215046584238339));
#12744=CARTESIAN_POINT('Ctrl Pts',(10.7381210493968,1.32201618867047,0.209534855263179));
#12745=CARTESIAN_POINT('Ctrl Pts',(10.7272598662103,1.31116338896628,0.416919242515175));
#12746=CARTESIAN_POINT('Ctrl Pts',(10.716398780155,1.30031077634578,0.624303643734563));
#12747=CARTESIAN_POINT('Ctrl Pts',(10.8001612475457,1.18151886169146,-0.00307678645922502));
#12748=CARTESIAN_POINT('Ctrl Pts',(10.7892926103682,1.17067663552019,0.20430785074418));
#12749=CARTESIAN_POINT('Ctrl Pts',(10.7784241800195,1.15983442267521,0.41169249890798));
#12750=CARTESIAN_POINT('Ctrl Pts',(10.7675555412906,1.14899250266155,0.619077151394146));
#12751=CARTESIAN_POINT('Ctrl Pts',(10.8003382383521,1.11671757294177,-0.00645397222975308));
#12752=CARTESIAN_POINT('Ctrl Pts',(10.7894696557425,1.1058798099729,0.200930938146656));
#12753=CARTESIAN_POINT('Ctrl Pts',(10.778601072647,1.09504222488243,0.408315857793383));
#12754=CARTESIAN_POINT('Ctrl Pts',(10.7677324890572,1.08420482079361,0.615700786872884));
#12755=CARTESIAN_POINT('Ctrl Pts',(10.5166159648474,1.4155315881283,3.37837396946483E-16));
#12756=CARTESIAN_POINT('Ctrl Pts',(10.5058777995597,1.40479094425298,0.205494164234944));
#12757=CARTESIAN_POINT('Ctrl Pts',(10.4951398148107,1.39405045994841,0.41098834481212));
#12758=CARTESIAN_POINT('Ctrl Pts',(10.4844020137689,1.3833101379008,0.616482542003833));
#12759=CARTESIAN_POINT('Ctrl Pts',(10.7677324890572,1.08420482079361,0.615700786872884));
#12760=CARTESIAN_POINT('Ctrl Pts',(10.7784883265195,1.09492980219801,0.410467182062988));
#12761=CARTESIAN_POINT('Ctrl Pts',(10.7892441634977,1.10565496086826,0.205233586491177));
#12762=CARTESIAN_POINT('Ctrl Pts',(10.8,1.11638029377732,-4.7271214720368E-17));
#12763=CARTESIAN_POINT('Ctrl Pts',(0.3318563713692,1.09142177001972,0.9));
#12764=CARTESIAN_POINT('Ctrl Pts',(1.77658538561441,1.20431139287985,0.9));
#12765=CARTESIAN_POINT('Ctrl Pts',(5.15852145577913,1.31798734362749,0.900000000000001));
#12766=CARTESIAN_POINT('Ctrl Pts',(8.53883158814675,1.18907590268945,0.9));
#12767=CARTESIAN_POINT('Ctrl Pts',(10.4681436286308,1.08420482079361,0.9));
#12768=CARTESIAN_POINT('Ctrl Pts',(0.325113511056836,1.17771496230318,0.9));
#12769=CARTESIAN_POINT('Ctrl Pts',(1.77238748853623,1.29094597754667,0.900005244311447));
#12770=CARTESIAN_POINT('Ctrl Pts',(5.15940689953628,1.40489117512763,0.899995532233175));
#12771=CARTESIAN_POINT('Ctrl Pts',(8.54259780483314,1.2757067056985,0.90000328531099));
#12772=CARTESIAN_POINT('Ctrl Pts',(10.4728449957889,1.17069581622255,0.9));
#12773=CARTESIAN_POINT('Ctrl Pts',(0.313425270489116,1.32729771265557,0.830156825336737));
#12774=CARTESIAN_POINT('Ctrl Pts',(1.76508272830699,1.44110107554431,0.829918234118879));
#12775=CARTESIAN_POINT('Ctrl Pts',(5.16095094050242,1.55552201031752,0.829677185710002));
#12776=CARTESIAN_POINT('Ctrl Pts',(8.54913632089268,1.4258591912674,0.829900861618366));
#12777=CARTESIAN_POINT('Ctrl Pts',(10.4809942371438,1.32061731204901,0.830050158657121));
#12778=CARTESIAN_POINT('Ctrl Pts',(0.308806004580394,1.38641375285276,0.681625057916928));
#12779=CARTESIAN_POINT('Ctrl Pts',(1.76222987578798,1.50017797416985,0.681006088930498));
#12780=CARTESIAN_POINT('Ctrl Pts',(5.16154986224672,1.61450132085358,0.68038246417749));
#12781=CARTESIAN_POINT('Ctrl Pts',(8.55170115551887,1.48491240850707,0.680961314820656));
#12782=CARTESIAN_POINT('Ctrl Pts',(10.4842082875648,1.37974615923803,0.681348425135383));
#12783=CARTESIAN_POINT('Ctrl Pts',(0.308522637995068,1.39004019713626,0.616809874278785));
#12784=CARTESIAN_POINT('Ctrl Pts',(1.76205965694675,1.50365920577193,0.616079089534579));
#12785=CARTESIAN_POINT('Ctrl Pts',(5.16158497046229,1.61783515152865,0.615338844765104));
#12786=CARTESIAN_POINT('Ctrl Pts',(8.55185322351876,1.48838233768137,0.616025627991778));
#12787=CARTESIAN_POINT('Ctrl Pts',(10.4844020137689,1.3833101379008,0.616482542003833));
#12788=CARTESIAN_POINT('Ctrl Pts',(10.4844020137689,1.3833101379008,0.616482542003833));
#12789=CARTESIAN_POINT('Ctrl Pts',(8.55185322351876,1.48838233768137,0.616025627991778));
#12790=CARTESIAN_POINT('Ctrl Pts',(5.16158497046229,1.61783515152865,0.615338844765104));
#12791=CARTESIAN_POINT('Ctrl Pts',(1.76205965694675,1.50365920577193,0.616079089534579));
#12792=CARTESIAN_POINT('Ctrl Pts',(0.308522637995068,1.39004019713626,0.616809874278785));
#12793=CARTESIAN_POINT('Ctrl Pts',(0.3318563713692,1.09142177001972,0.9));
#12794=CARTESIAN_POINT('Ctrl Pts',(1.77658538561441,1.20431139287985,0.9));
#12795=CARTESIAN_POINT('Ctrl Pts',(5.15852145577913,1.31798734362749,0.900000000000001));
#12796=CARTESIAN_POINT('Ctrl Pts',(8.53883158814675,1.18907590268945,0.9));
#12797=CARTESIAN_POINT('Ctrl Pts',(10.4681436286308,1.08420482079361,0.9));
#12798=CARTESIAN_POINT('Ctrl Pts',(-0.000344602063817145,1.12390349461883,
-0.00657539908256866));
#12799=CARTESIAN_POINT('Ctrl Pts',(0.0105261016091243,1.11307601020539,
0.200849983592616));
#12800=CARTESIAN_POINT('Ctrl Pts',(0.0213968059409475,1.10224876730309,
0.408275378840013));
#12801=CARTESIAN_POINT('Ctrl Pts',(0.0322675109428289,1.09142177001972,
0.615700786872884));
#12802=CARTESIAN_POINT('Ctrl Pts',(-0.000112549170678945,1.2089618047365,
-0.00214756610981592));
#12803=CARTESIAN_POINT('Ctrl Pts',(0.0107584275574203,1.19812589474889,
0.205277296000037));
#12804=CARTESIAN_POINT('Ctrl Pts',(0.021628504370896,1.18729063034778,0.412702239156743));
#12805=CARTESIAN_POINT('Ctrl Pts',(0.0324994852542487,1.17645511229507,
0.620127120417125));
#12806=CARTESIAN_POINT('Ctrl Pts',(0.0675181008536004,1.35659180908255,
0.00201426213057289));
#12807=CARTESIAN_POINT('Ctrl Pts',(0.0783748317004002,1.34574224493831,
0.20943904356877));
#12808=CARTESIAN_POINT('Ctrl Pts',(0.0892318011706237,1.33489254525337,
0.416863803530356));
#12809=CARTESIAN_POINT('Ctrl Pts',(0.100088380073201,1.32404321751407,0.624288602298589));
#12810=CARTESIAN_POINT('Ctrl Pts',(0.212439875011655,1.41741816253371,-0.00240566592686199));
#12811=CARTESIAN_POINT('Ctrl Pts',(0.223274062163905,1.40657840226088,0.20502076110302));
#12812=CARTESIAN_POINT('Ctrl Pts',(0.234108278795672,1.39573903465802,0.412447205628077));
#12813=CARTESIAN_POINT('Ctrl Pts',(0.244942059060342,1.38489960928785,0.619873667633733));
#12814=CARTESIAN_POINT('Ctrl Pts',(0.276041299849618,1.42253242682652,-0.00547191373834488));
#12815=CARTESIAN_POINT('Ctrl Pts',(0.286868655882245,1.41170146982041,0.201955326984501));
#12816=CARTESIAN_POINT('Ctrl Pts',(0.297695769965166,1.40087072543886,0.409382589539965));
#12817=CARTESIAN_POINT('Ctrl Pts',(0.308522637995069,1.39004019713626,0.616809874278785));
#12818=CARTESIAN_POINT('Ctrl Pts',(2.26869304592592E-17,1.12356026268968,
-3.16587034365767E-17));
#12819=CARTESIAN_POINT('Ctrl Pts',(0.0107558363321878,1.11284719399672,
0.205233583245308));
#12820=CARTESIAN_POINT('Ctrl Pts',(0.0215116733095221,1.10213436178043,
0.410467178800746));
#12821=CARTESIAN_POINT('Ctrl Pts',(0.0322675109428289,1.09142177001972,
0.615700786872884));
#12822=CARTESIAN_POINT('Ctrl Pts',(0.308522637995069,1.39004019713626,0.616809874278785));
#12823=CARTESIAN_POINT('Ctrl Pts',(0.297790973931072,1.40077548928706,0.411206561171438));
#12824=CARTESIAN_POINT('Ctrl Pts',(0.287059068122271,1.41151099373341,0.205603269859031));
#12825=CARTESIAN_POINT('Ctrl Pts',(0.276326924564681,1.42224670711126,-2.68882138776405E-16));
#12826=CARTESIAN_POINT('Ctrl Pts',(10.5166159648474,-1.4155315881283,0.));
#12827=CARTESIAN_POINT('Ctrl Pts',(10.5064062201588,-1.40475637621136,0.205603291426271));
#12828=CARTESIAN_POINT('Ctrl Pts',(10.4961964754701,-1.39398116429443,0.411206582852543));
#12829=CARTESIAN_POINT('Ctrl Pts',(10.4859867307814,-1.38320595237749,0.616809874278814));
#12830=CARTESIAN_POINT('Ctrl Pts',(7.10318628475318,-1.599994843061,0.));
#12831=CARTESIAN_POINT('Ctrl Pts',(7.09978773046573,-1.58921963114407,0.205603291426271));
#12832=CARTESIAN_POINT('Ctrl Pts',(7.09638917617828,-1.57844441922713,0.411206582852543));
#12833=CARTESIAN_POINT('Ctrl Pts',(7.09299062189083,-1.5676692073102,0.616809874278814));
#12834=CARTESIAN_POINT('Ctrl Pts',(3.68975660465893,-1.68747752195839,0.));
#12835=CARTESIAN_POINT('Ctrl Pts',(3.69316924077269,-1.67670231004145,0.205603291426272));
#12836=CARTESIAN_POINT('Ctrl Pts',(3.69658187688646,-1.66592709812452,0.411206582852543));
#12837=CARTESIAN_POINT('Ctrl Pts',(3.69999451300023,-1.65515188620758,0.616809874278814));
#12838=CARTESIAN_POINT('Ctrl Pts',(0.276326924564679,-1.42224670711126,
0.));
#12839=CARTESIAN_POINT('Ctrl Pts',(0.286550751079662,-1.41147149519433,
0.205603291426271));
#12840=CARTESIAN_POINT('Ctrl Pts',(0.296774577594646,-1.40069628327739,
0.411206582852543));
#12841=CARTESIAN_POINT('Ctrl Pts',(0.306998404109629,-1.38992107136046,
0.616809874278814));
#12842=CARTESIAN_POINT('Origin',(0.,-1.4,0.));
#12843=CARTESIAN_POINT('Origin',(5.4,-8.13935059369636E-18,0.9));
#12844=CARTESIAN_POINT('Ctrl Pts',(0.276326924564679,1.42224670711126,0.));
#12845=CARTESIAN_POINT('Ctrl Pts',(0.286550751079662,1.41147149519433,0.205603291426271));
#12846=CARTESIAN_POINT('Ctrl Pts',(0.296774577594645,1.40069628327739,0.411206582852543));
#12847=CARTESIAN_POINT('Ctrl Pts',(0.306998404109628,1.38992107136046,0.616809874278814));
#12848=CARTESIAN_POINT('Ctrl Pts',(3.68975660465893,1.68747752195839,0.));
#12849=CARTESIAN_POINT('Ctrl Pts',(3.6931692407727,1.67670231004145,0.205603291426271));
#12850=CARTESIAN_POINT('Ctrl Pts',(3.69658187688646,1.66592709812452,0.411206582852543));
#12851=CARTESIAN_POINT('Ctrl Pts',(3.69999451300023,1.65515188620758,0.616809874278814));
#12852=CARTESIAN_POINT('Ctrl Pts',(7.10318628475318,1.599994843061,0.));
#12853=CARTESIAN_POINT('Ctrl Pts',(7.09978773046573,1.58921963114407,0.205603291426271));
#12854=CARTESIAN_POINT('Ctrl Pts',(7.09638917617828,1.57844441922713,0.411206582852543));
#12855=CARTESIAN_POINT('Ctrl Pts',(7.09299062189083,1.5676692073102,0.616809874278814));
#12856=CARTESIAN_POINT('Ctrl Pts',(10.5166159648474,1.4155315881283,0.));
#12857=CARTESIAN_POINT('Ctrl Pts',(10.5064062201588,1.40475637621136,0.205603291426271));
#12858=CARTESIAN_POINT('Ctrl Pts',(10.4961964754701,1.39398116429443,0.411206582852543));
#12859=CARTESIAN_POINT('Ctrl Pts',(10.4859867307814,1.38320595237749,0.616809874278814));
#12860=CARTESIAN_POINT('Origin',(10.8,1.4,0.));
#12861=CARTESIAN_POINT('',(0.,0.,0.));
#12862=CARTESIAN_POINT('Origin',(0.,0.,0.));
#12863=CARTESIAN_POINT('',(-0.14652705620645,9.44412402177196E-5,0.0160655045842905));
#12864=CARTESIAN_POINT('',(-0.146479946776166,0.000162062070299865,0.00893449541571059));
#12865=CARTESIAN_POINT('',(-0.14635,-1.79227059055215E-17,0.));
#12866=CARTESIAN_POINT('',(0.0634007094575209,0.131904027763685,0.));
#12867=CARTESIAN_POINT('Ctrl Pts',(-0.14652705620645,9.44412402177196E-5,
0.0160655045842905));
#12868=CARTESIAN_POINT('Ctrl Pts',(-0.146560923555419,0.00502618404349199,
0.0157963945919035));
#12869=CARTESIAN_POINT('Ctrl Pts',(-0.146333578783787,0.00995455679532004,
0.0155272845995164));
#12870=CARTESIAN_POINT('Ctrl Pts',(-0.14583475180505,0.0148550342388422,
0.0152581746071293));
#12871=CARTESIAN_POINT('Ctrl Pts',(-0.140929468554047,0.0630445487404258,
0.0126118447280274));
#12872=CARTESIAN_POINT('Ctrl Pts',(-0.10977174472993,0.108536575508351,
0.0099655148489255));
#12873=CARTESIAN_POINT('Ctrl Pts',(-0.0666135938566871,0.13056551637767,
0.00731918496982359));
#12874=CARTESIAN_POINT('Ctrl Pts',(-0.0268248419338395,0.150874636338504,
0.00487945664654906));
#12875=CARTESIAN_POINT('Ctrl Pts',(0.0231637104697219,0.151241233100125,
0.00243972832327453));
#12876=CARTESIAN_POINT('Ctrl Pts',(0.0635546915223951,0.132092229195826,
-2.16840434497101E-19));
#12877=CARTESIAN_POINT('',(-0.0634007094575146,0.131904027763688,0.));
#12878=CARTESIAN_POINT('Origin',(0.,0.,0.));
#12879=CARTESIAN_POINT('Ctrl Pts',(-0.0634007094575145,0.131904027763688,
-3.88578058618805E-16));
#12880=CARTESIAN_POINT('Ctrl Pts',(-0.107282641710421,0.110811831533068,
0.00264738937425961));
#12881=CARTESIAN_POINT('Ctrl Pts',(-0.139432201149969,0.0662847592091173,
0.00529477874851962));
#12882=CARTESIAN_POINT('Ctrl Pts',(-0.145436119191498,0.0182745223106641,
0.00794216812277962));
#12883=CARTESIAN_POINT('Ctrl Pts',(-0.146186273512714,0.0122759249909008,
0.00827294388708994));
#12884=CARTESIAN_POINT('Ctrl Pts',(-0.146528267289359,0.00622295186417552,
0.00860371965140026));
#12885=CARTESIAN_POINT('Ctrl Pts',(-0.146479946776166,0.000162062070299865,
0.00893449541571059));
#12886=CARTESIAN_POINT('Origin',(0.,0.,0.));
#12887=CARTESIAN_POINT('',(-0.146148830924315,7.59978318484386E-5,0.0660655045842905));
#12888=CARTESIAN_POINT('',(-0.146133770585873,6.2751561688711E-5,0.0589344954157103));
#12889=CARTESIAN_POINT('',(-0.14635,-1.79227059055215E-17,0.));
#12890=CARTESIAN_POINT('Ctrl Pts',(-0.146148830924315,7.59978318484386E-5,
0.0660655045842905));
#12891=CARTESIAN_POINT('Ctrl Pts',(-0.146240443598182,0.0195917497831913,
0.0650077071998482));
#12892=CARTESIAN_POINT('Ctrl Pts',(-0.142607114239671,0.0390747476468127,
0.0639499098154059));
#12893=CARTESIAN_POINT('Ctrl Pts',(-0.135087779856993,0.056920264102034,
0.0628921124309636));
#12894=CARTESIAN_POINT('Ctrl Pts',(-0.116276389754784,0.10156503643559,
0.0602457825518617));
#12895=CARTESIAN_POINT('Ctrl Pts',(-0.073143724514267,0.135961331060063,
0.0575994526727599));
#12896=CARTESIAN_POINT('Ctrl Pts',(-0.025432083612881,0.144366623974243,
0.054953122793658));
#12897=CARTESIAN_POINT('Ctrl Pts',(0.0222795572885053,0.152771916888423,
0.0523067929145561));
#12898=CARTESIAN_POINT('Ctrl Pts',(0.0745701738507606,0.135186208092309,
0.0496604630354541));
#12899=CARTESIAN_POINT('Ctrl Pts',(0.107505148494886,0.0996564726649905,
0.0470141331563522));
#12900=CARTESIAN_POINT('Ctrl Pts',(0.140440123139012,0.0641267372376721,
0.0443678032772503));
#12901=CARTESIAN_POINT('Ctrl Pts',(0.154019455865009,0.010652975179149,
0.0417214733981484));
#12902=CARTESIAN_POINT('Ctrl Pts',(0.14202839331759,-0.0362847016460775,
0.0390751435190465));
#12903=CARTESIAN_POINT('Ctrl Pts',(0.130037330770172,-0.0832223784713041,
0.0364288136399446));
#12904=CARTESIAN_POINT('Ctrl Pts',(0.0924758729493388,-0.123623970063234,
0.0337824837608427));
#12905=CARTESIAN_POINT('Ctrl Pts',(0.0465351214488668,-0.139005253038876,
0.0311361538817407));
#12906=CARTESIAN_POINT('Ctrl Pts',(0.000594369948394902,-0.154386536014517,
0.0284898240026388));
#12907=CARTESIAN_POINT('Ctrl Pts',(-0.0537256752317158,-0.144747510373871,
0.025843494123537));
#12908=CARTESIAN_POINT('Ctrl Pts',(-0.0915592764828275,-0.114484496435928,
0.0231971642444351));
#12909=CARTESIAN_POINT('Ctrl Pts',(-0.125545511528741,-0.0872989822136326,
0.0208199443577202));
#12910=CARTESIAN_POINT('Ctrl Pts',(-0.146227884351973,-0.0434707826450544,
0.0184427244710054));
#12911=CARTESIAN_POINT('Ctrl Pts',(-0.14652705620645,9.44412402177196E-5,
0.0160655045842905));
#12912=CARTESIAN_POINT('Ctrl Pts',(-0.146479946776166,0.000162062070299865,
0.00893449541571059));
#12913=CARTESIAN_POINT('Ctrl Pts',(-0.146141530330399,-0.0422858476614564,
0.0112511090256603));
#12914=CARTESIAN_POINT('Ctrl Pts',(-0.126658161292025,-0.0851220706608281,
0.0135677226356099));
#12915=CARTESIAN_POINT('Ctrl Pts',(-0.0941604943243988,-0.112386678841155,
0.0158843362455596));
#12916=CARTESIAN_POINT('Ctrl Pts',(-0.0570226747722624,-0.143544241621566,
0.0185317256198196));
#12917=CARTESIAN_POINT('Ctrl Pts',(-0.00288875902448078,-0.154365965709432,
0.0211791149940796));
#12918=CARTESIAN_POINT('Ctrl Pts',(0.0434083729543798,-0.140002007265973,
0.0238265043683396));
#12919=CARTESIAN_POINT('Ctrl Pts',(0.0897055049332404,-0.125638048822514,
0.0264738937425996));
#12920=CARTESIAN_POINT('Ctrl Pts',(0.12816585314318,-0.0860884078477292,
0.0291212831168596));
#12921=CARTESIAN_POINT('Ctrl Pts',(0.141191617966992,-0.0394144013492358,
0.0317686724911196));
#12922=CARTESIAN_POINT('Ctrl Pts',(0.154217382790803,0.00725960514925768,
0.0344160618653796));
#12923=CARTESIAN_POINT('Ctrl Pts',(0.141808564228487,0.0610579771714599,
0.0370634512396396));
#12924=CARTESIAN_POINT('Ctrl Pts',(0.109639063769471,0.0973098477439542,
0.0397108406138996));
#12925=CARTESIAN_POINT('Ctrl Pts',(0.0774695633104545,0.133561718316448,
0.0423582299881596));
#12926=CARTESIAN_POINT('Ctrl Pts',(0.0255393809547383,0.152267087439235,
0.0450056193624196));
#12927=CARTESIAN_POINT('Ctrl Pts',(-0.0223595433272462,0.144872892294413,
0.0476530087366796));
#12928=CARTESIAN_POINT('Ctrl Pts',(-0.070258467609231,0.137478697149591,
0.0503003981109396));
#12929=CARTESIAN_POINT('Ctrl Pts',(-0.114126133817484,0.10398493773716,
0.0529477874851996));
#12930=CARTESIAN_POINT('Ctrl Pts',(-0.133871661545403,0.059725601630819,
0.0555951768594596));
#12931=CARTESIAN_POINT('Ctrl Pts',(-0.142173753131161,0.0411165744656389,
0.0567082830448765));
#12932=CARTESIAN_POINT('Ctrl Pts',(-0.146211489678532,0.0206043892842972,
0.0578213892302934));
#12933=CARTESIAN_POINT('Ctrl Pts',(-0.146133770585873,6.2751561688711E-5,
0.0589344954157103));
#12934=CARTESIAN_POINT('Origin',(0.,0.,0.));
#12935=CARTESIAN_POINT('',(-0.146252097264499,-0.000124487410312429,0.116065504584291));
#12936=CARTESIAN_POINT('',(-0.146276374479508,-0.000129480650117819,0.10893449541571));
#12937=CARTESIAN_POINT('',(-0.14635,-1.79227059055215E-17,0.));
#12938=CARTESIAN_POINT('Ctrl Pts',(-0.146252097264499,-0.000124487410312429,
0.116065504584291));
#12939=CARTESIAN_POINT('Ctrl Pts',(-0.145977101830714,0.0338815411246725,
0.114219019807793));
#12940=CARTESIAN_POINT('Ctrl Pts',(-0.134160879762789,0.0680598926014691,
0.112372535031295));
#12941=CARTESIAN_POINT('Ctrl Pts',(-0.112484833627769,0.0939988017516943,
0.110526050254798));
#12942=CARTESIAN_POINT('Ctrl Pts',(-0.0814193359437304,0.131173714423195,
0.107879720375696));
#12943=CARTESIAN_POINT('Ctrl Pts',(-0.0301019434218634,0.151424966146533,
0.105233390496594));
#12944=CARTESIAN_POINT('Ctrl Pts',(0.0179785702873004,0.145483266051774,
0.102587060617492));
#12945=CARTESIAN_POINT('Ctrl Pts',(0.0660590839964643,0.139541565957016,
0.0999407307383904));
#12946=CARTESIAN_POINT('Ctrl Pts',(0.110902718892925,0.107406914044162,
0.0972944008592884));
#12947=CARTESIAN_POINT('Ctrl Pts',(0.131983829661647,0.0637877973597534,
0.0946480709801865));
#12948=CARTESIAN_POINT('Ctrl Pts',(0.15306494043037,0.0201686806753445,
0.0920017411010846));
#12949=CARTESIAN_POINT('Ctrl Pts',(0.150383527071356,-0.0349349007806195,
0.0893554112219828));
#12950=CARTESIAN_POINT('Ctrl Pts',(0.125166930059577,-0.0763010783846813,
0.0867090813428809));
#12951=CARTESIAN_POINT('Ctrl Pts',(0.0999503330477985,-0.117667255988743,
0.084062751463779));
#12952=CARTESIAN_POINT('Ctrl Pts',(0.0521985523832557,-0.145296029740903,
0.081416421584677));
#12953=CARTESIAN_POINT('Ctrl Pts',(0.00376830011669856,-0.146541450754272,
0.0787700917055751));
#12954=CARTESIAN_POINT('Ctrl Pts',(-0.0446619521498586,-0.147786871767642,
0.0761237618264732));
#12955=CARTESIAN_POINT('Ctrl Pts',(-0.09377067601843,-0.122648940042221,
0.0734774319473713));
#12956=CARTESIAN_POINT('Ctrl Pts',(-0.121079980470766,-0.0826333491581908,
0.0708311020682694));
#12957=CARTESIAN_POINT('Ctrl Pts',(-0.137473143648068,-0.0586128871159229,
0.0692425695736098));
#12958=CARTESIAN_POINT('Ctrl Pts',(-0.146011252866834,-0.02923151094855,
0.0676540370789502));
#12959=CARTESIAN_POINT('Ctrl Pts',(-0.146148830924315,7.59978318484386E-5,
0.0660655045842905));
#12960=CARTESIAN_POINT('Ctrl Pts',(-0.146133770585873,6.2751561688711E-5,
0.0589344954157103));
#12961=CARTESIAN_POINT('Ctrl Pts',(-0.146026644150963,-0.0282514289199324,
0.0604687786045534));
#12962=CARTESIAN_POINT('Ctrl Pts',(-0.138100435392092,-0.0566215672018456,
0.0620030617933965));
#12963=CARTESIAN_POINT('Ctrl Pts',(-0.122745086057252,-0.0801407530065182,
0.0635373449822396));
#12964=CARTESIAN_POINT('Ctrl Pts',(-0.0962495935935968,-0.120722858737265,
0.0661847343564996));
#12965=CARTESIAN_POINT('Ctrl Pts',(-0.0476352194187008,-0.146862157398507,
0.0688321237307596));
#12966=CARTESIAN_POINT('Ctrl Pts',(0.00082938917649622,-0.146587691816784,
0.0714795131050196));
#12967=CARTESIAN_POINT('Ctrl Pts',(0.0492939977716932,-0.146313226235061,
0.0741269024792796));
#12968=CARTESIAN_POINT('Ctrl Pts',(0.0976088407871913,-0.119624996410372,
0.0767742918535397));
#12969=CARTESIAN_POINT('Ctrl Pts',(0.123643642180798,-0.0787464320231966,
0.0794216812277997));
#12970=CARTESIAN_POINT('Ctrl Pts',(0.149678443574405,-0.0378678676360213,
0.0820690706020596));
#12971=CARTESIAN_POINT('Ctrl Pts',(0.153433203346121,0.0172010313136401,
0.0847164599763195));
#12972=CARTESIAN_POINT('Ctrl Pts',(0.133187835944515,0.06123527443138,0.0873638493505795));
#12973=CARTESIAN_POINT('Ctrl Pts',(0.11294246854291,0.10526951754912,0.0900112387248395));
#12974=CARTESIAN_POINT('Ctrl Pts',(0.0686969739679828,0.138269104834938,
0.0926586280990997));
#12975=CARTESIAN_POINT('Ctrl Pts',(0.0207181735233275,0.145118849380084,
0.0953060174733597));
#12976=CARTESIAN_POINT('Ctrl Pts',(-0.027260626921328,0.151968593925229,
0.0979534068476197));
#12977=CARTESIAN_POINT('Ctrl Pts',(-0.0789727332357116,0.132668495729702,
0.10060079622188));
#12978=CARTESIAN_POINT('Ctrl Pts',(-0.110731403441959,0.0960588230543748,
0.10324818559614));
#12979=CARTESIAN_POINT('Ctrl Pts',(-0.133469481440122,0.0698475998711364,
0.105143622202663));
#12980=CARTESIAN_POINT('Ctrl Pts',(-0.145979327216774,0.0347634013028336,
0.107039058809187));
#12981=CARTESIAN_POINT('Ctrl Pts',(-0.146276374479508,-0.000129480650117819,
0.10893449541571));
#12982=CARTESIAN_POINT('Origin',(0.,0.,0.));
#12983=CARTESIAN_POINT('',(-0.146589818999335,-3.81787486967988E-6,0.166065504584291));
#12984=CARTESIAN_POINT('',(-0.146589453522336,1.04004190909306E-5,0.15893449541571));
#12985=CARTESIAN_POINT('',(-0.14635,-1.79227059055215E-17,0.));
#12986=CARTESIAN_POINT('Ctrl Pts',(-0.146589818999335,-3.81787486967988E-6,
0.166065504584291));
#12987=CARTESIAN_POINT('Ctrl Pts',(-0.146571339149733,0.0482382848470949,
0.163430332415738));
#12988=CARTESIAN_POINT('Ctrl Pts',(-0.120433071521034,0.0964975486977609,
0.160795160247185));
#12989=CARTESIAN_POINT('Ctrl Pts',(-0.0800107885095625,0.122828684230981,
0.158159988078632));
#12990=CARTESIAN_POINT('Ctrl Pts',(-0.0394173515450545,0.149271309704865,
0.15551365819953));
#12991=CARTESIAN_POINT('Ctrl Pts',(0.0155813181737399,0.153599719825856,
0.152867328320428));
#12992=CARTESIAN_POINT('Ctrl Pts',(0.0598114643267532,0.133832733731537,
0.150220998441327));
#12993=CARTESIAN_POINT('Ctrl Pts',(0.104041610479766,0.114065747637217,
0.147574668562225));
#12994=CARTESIAN_POINT('Ctrl Pts',(0.137503233066998,0.0702033653275883,
0.144928338683123));
#12995=CARTESIAN_POINT('Ctrl Pts',(0.144880420813362,0.0223220882221681,
0.142282008804021));
#12996=CARTESIAN_POINT('Ctrl Pts',(0.152257608559726,-0.0255591888832524,
0.139635678924919));
#12997=CARTESIAN_POINT('Ctrl Pts',(0.133550361465222,-0.077459360784464,
0.136989349045817));
#12998=CARTESIAN_POINT('Ctrl Pts',(0.0973212811704284,-0.109622900294719,
0.134343019166715));
#12999=CARTESIAN_POINT('Ctrl Pts',(0.0610922008756344,-0.141786439804975,
0.131696689287613));
#13000=CARTESIAN_POINT('Ctrl Pts',(0.00734128738055008,-0.154213346924274,
0.129050359408511));
#13001=CARTESIAN_POINT('Ctrl Pts',(-0.0393288211819405,-0.141215634503184,
0.126404029529409));
#13002=CARTESIAN_POINT('Ctrl Pts',(-0.0859989297444312,-0.128217922082094,
0.123757699650308));
#13003=CARTESIAN_POINT('Ctrl Pts',(-0.125588233374328,-0.0897955901206149,
0.121111369771206));
#13004=CARTESIAN_POINT('Ctrl Pts',(-0.139976083766172,-0.043535137330043,
0.118465039892104));
#13005=CARTESIAN_POINT('Ctrl Pts',(-0.144324767489921,-0.0295530571287048,
0.117665194789499));
#13006=CARTESIAN_POINT('Ctrl Pts',(-0.146371217526823,-0.0148549394177889,
0.116865349686895));
#13007=CARTESIAN_POINT('Ctrl Pts',(-0.146252097264499,-0.000124487410312429,
0.116065504584291));
#13008=CARTESIAN_POINT('Ctrl Pts',(-0.146276374479508,-0.000129480650117819,
0.10893449541571));
#13009=CARTESIAN_POINT('Ctrl Pts',(-0.14639421831063,-0.0139720956278579,
0.109686448183447));
#13010=CARTESIAN_POINT('Ctrl Pts',(-0.14458995413065,-0.0277846002915201,
0.110438400951183));
#13011=CARTESIAN_POINT('Ctrl Pts',(-0.140739671041232,-0.041001045008257,
0.11119035371892));
#13012=CARTESIAN_POINT('Ctrl Pts',(-0.127184034336146,-0.0875319932404337,
0.11383774309318));
#13013=CARTESIAN_POINT('Ctrl Pts',(-0.0882675268278623,-0.12667464254966,
0.11648513246744));
#13014=CARTESIAN_POINT('Ctrl Pts',(-0.0418159243469935,-0.140499695546946,
0.1191325218417));
#13015=CARTESIAN_POINT('Ctrl Pts',(0.00463567813387508,-0.154324748544231,
0.12177991121596));
#13016=CARTESIAN_POINT('Ctrl Pts',(0.0586223755873289,-0.142832205229577,
0.12442730059022));
#13017=CARTESIAN_POINT('Ctrl Pts',(0.0954154960694136,-0.111286216216264,
0.12707468996448));
#13018=CARTESIAN_POINT('Ctrl Pts',(0.132208616551499,-0.0797402272029501,
0.12972207933874));
#13019=CARTESIAN_POINT('Ctrl Pts',(0.151808160062214,-0.0281407924909768,
0.132369468712999));
#13020=CARTESIAN_POINT('Ctrl Pts',(0.145236524363737,0.0198768833792122,
0.135016858087259));
#13021=CARTESIAN_POINT('Ctrl Pts',(0.138664888665259,0.0678945592494009,
0.13766424746152));
#13022=CARTESIAN_POINT('Ctrl Pts',(0.105922073757589,0.112330476277805,
0.14031163683578));
#13023=CARTESIAN_POINT('Ctrl Pts',(0.062005973158836,0.132830708741579,
0.14295902621004));
#13024=CARTESIAN_POINT('Ctrl Pts',(0.0180898725600832,0.153330941205352,
0.1456064155843));
#13025=CARTESIAN_POINT('Ctrl Pts',(-0.0369995137297515,0.149895489104495,
0.14825380495856));
#13026=CARTESIAN_POINT('Ctrl Pts',(-0.0780284182758478,0.124097962381086,
0.15090119433282));
#13027=CARTESIAN_POINT('Ctrl Pts',(-0.119057322821944,0.0983004356576776,
0.153548583707079));
#13028=CARTESIAN_POINT('Ctrl Pts',(-0.146025745624302,0.0501408343117172,
0.15619597308134));
#13029=CARTESIAN_POINT('Ctrl Pts',(-0.14658076309025,0.00167873146180186,
0.1588433624556));
#13030=CARTESIAN_POINT('Ctrl Pts',(-0.146587131676737,0.00112264969450139,
0.15887374010897));
#13031=CARTESIAN_POINT('Ctrl Pts',(-0.146590022522527,0.000566528098114988,
0.15890411776234));
#13032=CARTESIAN_POINT('Ctrl Pts',(-0.146589453522336,1.04004190909306E-5,
0.15893449541571));
#13033=CARTESIAN_POINT('Origin',(0.,0.,0.));
#13034=CARTESIAN_POINT('',(-0.146263250741535,0.000126870157254357,0.21606550458429));
#13035=CARTESIAN_POINT('',(-0.146245769975643,0.000123264779366826,0.20893449541571));
#13036=CARTESIAN_POINT('',(-0.14635,-1.79227059055215E-17,0.));
#13037=CARTESIAN_POINT('Ctrl Pts',(-0.146263250741535,0.000126870157254357,
0.21606550458429));
#13038=CARTESIAN_POINT('Ctrl Pts',(-0.146381923100139,0.0144435832128767,
0.215287974902784));
#13039=CARTESIAN_POINT('Ctrl Pts',(-0.144450237714319,0.0287289633064517,
0.214510445221278));
#13040=CARTESIAN_POINT('Ctrl Pts',(-0.140337374518256,0.0423560295890773,
0.213732915539772));
#13041=CARTESIAN_POINT('Ctrl Pts',(-0.126339204386259,0.0887358830222778,
0.21108658566067));
#13042=CARTESIAN_POINT('Ctrl Pts',(-0.0870745347363382,0.127489909020004,
0.208440255781569));
#13043=CARTESIAN_POINT('Ctrl Pts',(-0.0405154226099946,0.140879780169064,
0.205793925902467));
#13044=CARTESIAN_POINT('Ctrl Pts',(0.00604368951634975,0.154269651318124,
0.203147596023365));
#13045=CARTESIAN_POINT('Ctrl Pts',(0.0598972441191175,0.142295367618517,
0.200501266144263));
#13046=CARTESIAN_POINT('Ctrl Pts',(0.0963956219934077,0.110437747119808,
0.197854936265161));
#13047=CARTESIAN_POINT('Ctrl Pts',(0.132893999867697,0.0785801266211,0.195208606386059));
#13048=CARTESIAN_POINT('Ctrl Pts',(0.15203720101351,0.0268391693232909,
0.192562276506957));
#13049=CARTESIAN_POINT('Ctrl Pts',(0.145063081087281,-0.0211024746124516,
0.189915946627855));
#13050=CARTESIAN_POINT('Ctrl Pts',(0.138088961161051,-0.0690441185481943,
0.187269616748753));
#13051=CARTESIAN_POINT('Ctrl Pts',(0.10499752016278,-0.11318644912187,0.184623286869651));
#13052=CARTESIAN_POINT('Ctrl Pts',(0.060935231264163,-0.133324827106958,
0.181976956990549));
#13053=CARTESIAN_POINT('Ctrl Pts',(0.0168729423655461,-0.153463205092045,
0.179330627111448));
#13054=CARTESIAN_POINT('Ctrl Pts',(-0.0381601944334158,-0.149597630488544,
0.176684297232346));
#13055=CARTESIAN_POINT('Ctrl Pts',(-0.0789746466099193,-0.123497437688695,
0.174037967353244));
#13056=CARTESIAN_POINT('Ctrl Pts',(-0.119961184605052,-0.0972871987457574,
0.171380479763593));
#13057=CARTESIAN_POINT('Ctrl Pts',(-0.146608455341797,-0.0486544490602708,
0.168722992173942));
#13058=CARTESIAN_POINT('Ctrl Pts',(-0.146589818999335,-3.81787486967988E-6,
0.166065504584291));
#13059=CARTESIAN_POINT('Ctrl Pts',(-0.146589453522336,1.04004190909306E-5,
0.15893449541571));
#13060=CARTESIAN_POINT('Ctrl Pts',(-0.146540434588914,-0.0478995759235739,
0.1615515071366));
#13061=CARTESIAN_POINT('Ctrl Pts',(-0.120813506558866,-0.0958546957256878,
0.16416851885749));
#13062=CARTESIAN_POINT('Ctrl Pts',(-0.0808500697395765,-0.122278388912248,
0.16678553057838));
#13063=CARTESIAN_POINT('Ctrl Pts',(-0.0404227467934142,-0.149008802082514,
0.16943291995264));
#13064=CARTESIAN_POINT('Ctrl Pts',(0.0145735112284506,-0.153705024069172,
0.1720803093269));
#13065=CARTESIAN_POINT('Ctrl Pts',(0.0589475933459444,-0.134215943447351,
0.17472769870116));
#13066=CARTESIAN_POINT('Ctrl Pts',(0.103321675463438,-0.11472686282553,
0.17737508807542));
#13067=CARTESIAN_POINT('Ctrl Pts',(0.137073581676561,-0.0710524795952304,
0.18002247744968));
#13068=CARTESIAN_POINT('Ctrl Pts',(0.144743205110219,-0.0231979049720499,
0.18266986682394));
#13069=CARTESIAN_POINT('Ctrl Pts',(0.152412828543877,0.024656669651131,
0.1853172561982));
#13070=CARTESIAN_POINT('Ctrl Pts',(0.13400016919807,0.0766914356671922,
0.18796464557246));
#13071=CARTESIAN_POINT('Ctrl Pts',(0.0979391709064228,0.109071797518936,
0.19061203494672));
#13072=CARTESIAN_POINT('Ctrl Pts',(0.0618781726147763,0.141452159370678,
0.19325942432098));
#13073=CARTESIAN_POINT('Ctrl Pts',(0.00816883537729064,0.154178117058104,
0.195906813695239));
#13074=CARTESIAN_POINT('Ctrl Pts',(-0.0385872054932313,0.1414205281901,
0.198554203069499));
#13075=CARTESIAN_POINT('Ctrl Pts',(-0.0853432463637543,0.128662939322095,
0.201201592443759));
#13076=CARTESIAN_POINT('Ctrl Pts',(-0.125145990867313,0.0904218038986596,
0.20384898181802));
#13077=CARTESIAN_POINT('Ctrl Pts',(-0.139763737461459,0.0442135263146365,
0.20649637119228));
#13078=CARTESIAN_POINT('Ctrl Pts',(-0.144251162244238,0.030028291356252,
0.207309079266757));
#13079=CARTESIAN_POINT('Ctrl Pts',(-0.146365162502875,0.0150922359825044,
0.208121787341234));
#13080=CARTESIAN_POINT('Ctrl Pts',(-0.146245769975643,0.000123264779366826,
0.20893449541571));
#13081=CARTESIAN_POINT('Origin',(0.,0.,0.));
#13082=CARTESIAN_POINT('',(-0.146142672279203,-7.01165389862951E-5,0.266065504584291));
#13083=CARTESIAN_POINT('',(-0.146150215784492,-7.74481165901552E-5,0.258934495415711));
#13084=CARTESIAN_POINT('',(-0.14635,-1.79227059055215E-17,0.));
#13085=CARTESIAN_POINT('Ctrl Pts',(-0.146142672279203,-7.01165389862951E-5,
0.266065504584291));
#13086=CARTESIAN_POINT('Ctrl Pts',(-0.146017527260215,0.028828671850369,
0.264499287510729));
#13087=CARTESIAN_POINT('Ctrl Pts',(-0.137733916992107,0.0577936173630845,
0.262933070437168));
#13088=CARTESIAN_POINT('Ctrl Pts',(-0.121770841384076,0.0816117278206753,
0.261366853363607));
#13089=CARTESIAN_POINT('Ctrl Pts',(-0.0947991242083451,0.121855560193383,
0.258720523484505));
#13090=CARTESIAN_POINT('Ctrl Pts',(-0.0459036471244643,0.147405924851771,
0.256074193605403));
#13091=CARTESIAN_POINT('Ctrl Pts',(0.0025353607453442,0.146568017913755,
0.253427863726301));
#13092=CARTESIAN_POINT('Ctrl Pts',(0.050974368615152,0.145730110975738,
0.250781533847199));
#13093=CARTESIAN_POINT('Ctrl Pts',(0.0989569072708876,0.118503932441319,
0.248135203968097));
#13094=CARTESIAN_POINT('Ctrl Pts',(0.124520613871998,0.0773513325689396,
0.245488874088995));
#13095=CARTESIAN_POINT('Ctrl Pts',(0.150084320473109,0.0361987326965595,
0.242842544209893));
#13096=CARTESIAN_POINT('Ctrl Pts',(0.153229195019594,-0.0188802885137813,
0.240196214330791));
#13097=CARTESIAN_POINT('Ctrl Pts',(0.132515778953886,-0.0626751965094481,
0.237549884451689));
#13098=CARTESIAN_POINT('Ctrl Pts',(0.111802362888177,-0.106470104505115,
0.234903554572587));
#13099=CARTESIAN_POINT('Ctrl Pts',(0.0672306562102751,-0.138980899286108,
0.232257224693486));
#13100=CARTESIAN_POINT('Ctrl Pts',(0.0192018303028616,-0.145326878595667,
0.229610894814384));
#13101=CARTESIAN_POINT('Ctrl Pts',(-0.0288269956045516,-0.151672857905225,
0.226964564935282));
#13102=CARTESIAN_POINT('Ctrl Pts',(-0.0803129407414762,-0.131854021743351,
0.22431823505618));
#13103=CARTESIAN_POINT('Ctrl Pts',(-0.111690078002902,-0.0949417632280756,
0.221671905177078));
#13104=CARTESIAN_POINT('Ctrl Pts',(-0.133848162215005,-0.0688748557907962,
0.219803104979482));
#13105=CARTESIAN_POINT('Ctrl Pts',(-0.145978020566425,-0.0342834897603843,
0.217934304781886));
#13106=CARTESIAN_POINT('Ctrl Pts',(-0.146263250741535,0.000126870157254357,
0.21606550458429));
#13107=CARTESIAN_POINT('Ctrl Pts',(-0.146245769975643,0.000123264779366826,
0.20893449541571));
#13108=CARTESIAN_POINT('Ctrl Pts',(-0.145976242399967,-0.03366905549635,
0.210769176715493));
#13109=CARTESIAN_POINT('Ctrl Pts',(-0.134324750276972,-0.067629123606452,
0.212603858015276));
#13110=CARTESIAN_POINT('Ctrl Pts',(-0.112902327433,-0.0934976078712483,
0.214438539315059));
#13111=CARTESIAN_POINT('Ctrl Pts',(-0.0819904221256615,-0.130825044728502,
0.217085928689319));
#13112=CARTESIAN_POINT('Ctrl Pts',(-0.0307338628262512,-0.151304498698398,
0.21973331806358));
#13113=CARTESIAN_POINT('Ctrl Pts',(0.0173892134168267,-0.145555327884408,
0.22238070743784));
#13114=CARTESIAN_POINT('Ctrl Pts',(0.0655122896599044,-0.139806157070418,
0.2250280968121));
#13115=CARTESIAN_POINT('Ctrl Pts',(0.11050188284665,-0.107828361472542,
0.22767548618636));
#13116=CARTESIAN_POINT('Ctrl Pts',(0.131750448317205,-0.0642694140823833,
0.23032287556062));
#13117=CARTESIAN_POINT('Ctrl Pts',(0.15299901378776,-0.020710466692225,
0.232970264934879));
#13118=CARTESIAN_POINT('Ctrl Pts',(0.150506551542124,0.0344296324902152,
0.23561765430914));
#13119=CARTESIAN_POINT('Ctrl Pts',(0.125414737320077,0.0758938856636754,
0.2382650436834));
#13120=CARTESIAN_POINT('Ctrl Pts',(0.10032292309803,0.117358138837136,0.24091243305766));
#13121=CARTESIAN_POINT('Ctrl Pts',(0.0526317568995709,0.145146546001616,
0.24355982243192));
#13122=CARTESIAN_POINT('Ctrl Pts',(0.00418624259284972,0.146530589268381,
0.24620721180618));
#13123=CARTESIAN_POINT('Ctrl Pts',(-0.0442592717138715,0.147914632535146,
0.24885460118044));
#13124=CARTESIAN_POINT('Ctrl Pts',(-0.0934591341288551,0.122894311904195,
0.2515019905547));
#13125=CARTESIAN_POINT('Ctrl Pts',(-0.120877280418781,0.082930219442967,
0.25414937992896));
#13126=CARTESIAN_POINT('Ctrl Pts',(-0.137396572682769,0.0588520590724165,
0.255744418424543));
#13127=CARTESIAN_POINT('Ctrl Pts',(-0.146009100715185,0.0293493086505574,
0.257339456920127));
#13128=CARTESIAN_POINT('Ctrl Pts',(-0.146150215784492,-7.74481165901552E-5,
0.258934495415711));
#13129=CARTESIAN_POINT('Origin',(0.,0.,0.));
#13130=CARTESIAN_POINT('',(-0.146519404976022,-8.97763884284003E-5,0.316065504584291));
#13131=CARTESIAN_POINT('',(-0.146528765763263,-8.45393868379275E-5,0.30893449541571));
#13132=CARTESIAN_POINT('',(-0.14635,-1.79227059055215E-17,0.));
#13133=CARTESIAN_POINT('Ctrl Pts',(-0.146519404976022,-8.97763884284003E-5,
0.316065504584291));
#13134=CARTESIAN_POINT('Ctrl Pts',(-0.146208092107557,0.043076445171776,
0.313710600118674));
#13135=CARTESIAN_POINT('Ctrl Pts',(-0.125958424314353,0.0864965766126209,
0.311355695653057));
#13136=CARTESIAN_POINT('Ctrl Pts',(-0.0925183485457987,0.1137056160074,
0.309000791187441));
#13137=CARTESIAN_POINT('Ctrl Pts',(-0.0549399784004991,0.144281843189175,
0.306354461308339));
#13138=CARTESIAN_POINT('Ctrl Pts',(-0.00070450021881692,0.154386382754941,
0.303708131429237));
#13139=CARTESIAN_POINT('Ctrl Pts',(0.0453636543616171,0.139394227973128,
0.301061801550135));
#13140=CARTESIAN_POINT('Ctrl Pts',(0.0914318089420511,0.124402073191315,
0.298415471671033));
#13141=CARTESIAN_POINT('Ctrl Pts',(0.129332639921237,0.0843132240619223,
0.295769141791931));
#13142=CARTESIAN_POINT('Ctrl Pts',(0.141718340675246,0.0374769775398043,
0.293122811912829));
#13143=CARTESIAN_POINT('Ctrl Pts',(0.154104041429255,-0.00935926898231351,
0.290476482033727));
#13144=CARTESIAN_POINT('Ctrl Pts',(0.140974611958088,-0.0629429128971569,
0.287830152154626));
#13145=CARTESIAN_POINT('Ctrl Pts',(0.108339598692885,-0.0987478773661917,
0.285183822275524));
#13146=CARTESIAN_POINT('Ctrl Pts',(0.0757045854276824,-0.134552841835227,
0.282537492396422));
#13147=CARTESIAN_POINT('Ctrl Pts',(0.0235639883684441,-0.152579126858453,
0.27989116251732));
#13148=CARTESIAN_POINT('Ctrl Pts',(-0.0242166208952047,-0.144575818177467,
0.277244832638218));
#13149=CARTESIAN_POINT('Ctrl Pts',(-0.0719972301588528,-0.136572509496481,
0.274598502759116));
#13150=CARTESIAN_POINT('Ctrl Pts',(-0.115417851626912,-0.102539607111283,
0.271952172880014));
#13151=CARTESIAN_POINT('Ctrl Pts',(-0.13460418372715,-0.0580545058751705,
0.269305843000912));
#13152=CARTESIAN_POINT('Ctrl Pts',(-0.142435181350113,-0.0398976888130428,
0.268225730195372));
#13153=CARTESIAN_POINT('Ctrl Pts',(-0.146228976240411,-0.0199996345674016,
0.267145617389831));
#13154=CARTESIAN_POINT('Ctrl Pts',(-0.146142672279203,-7.01165389862951E-5,
0.266065504584291));
#13155=CARTESIAN_POINT('Ctrl Pts',(-0.146150215784492,-7.74481165901552E-5,
0.258934495415711));
#13156=CARTESIAN_POINT('Ctrl Pts',(-0.146243318595233,-0.0194921979337541,
0.259986846294387));
#13157=CARTESIAN_POINT('Ctrl Pts',(-0.142648899141753,-0.0388738684647463,
0.261039197173063));
#13158=CARTESIAN_POINT('Ctrl Pts',(-0.135204796371803,-0.0566427511368837,
0.26209154805174));
#13159=CARTESIAN_POINT('Ctrl Pts',(-0.116477735870028,-0.101343764964001,
0.264738937426));
#13160=CARTESIAN_POINT('Ctrl Pts',(-0.0733871847016099,-0.135837928326728,
0.26738632680026));
#13161=CARTESIAN_POINT('Ctrl Pts',(-0.0256708287318585,-0.144325142544676,
0.27003371617452));
#13162=CARTESIAN_POINT('Ctrl Pts',(0.0220455272378925,-0.152812356762624,
0.27268110554878));
#13163=CARTESIAN_POINT('Ctrl Pts',(0.0743876880089763,-0.135292621835792,
0.27532849492304));
#13164=CARTESIAN_POINT('Ctrl Pts',(0.10738025529095,-0.0997908762961729,
0.2779758842973));
#13165=CARTESIAN_POINT('Ctrl Pts',(0.140372822572925,-0.0642891307565533,
0.280623273671559));
#13166=CARTESIAN_POINT('Ctrl Pts',(0.154015796365789,-0.010805374604146,
0.283270663045819));
#13167=CARTESIAN_POINT('Ctrl Pts',(0.142059993874458,0.0361620845457957,
0.285918052420079));
#13168=CARTESIAN_POINT('Ctrl Pts',(0.130104191383128,0.0831295436957373,
0.288565441794339));
#13169=CARTESIAN_POINT('Ctrl Pts',(0.0925496126076039,0.123580705843213,
0.291212831168599));
#13170=CARTESIAN_POINT('Ctrl Pts',(0.0465981836912963,0.138986860871753,
0.29386022054286));
#13171=CARTESIAN_POINT('Ctrl Pts',(0.000646754774988913,0.154393015900293,
0.296507609917119));
#13172=CARTESIAN_POINT('Ctrl Pts',(-0.0537015242821025,0.144754163809898,
0.29915499929138));
#13173=CARTESIAN_POINT('Ctrl Pts',(-0.0915523499663989,0.114485393976436,
0.30180238866564));
#13174=CARTESIAN_POINT('Ctrl Pts',(-0.125542580994678,0.0873038870745135,
0.30417975758233));
#13175=CARTESIAN_POINT('Ctrl Pts',(-0.146229051243382,0.0434861464246214,
0.30655712649902));
#13176=CARTESIAN_POINT('Ctrl Pts',(-0.146528765763263,-8.45393868379275E-5,
0.30893449541571));
#13177=CARTESIAN_POINT('Origin',(0.,0.,0.));
#13178=CARTESIAN_POINT('',(-0.146416087288192,0.000126442170093593,0.366065504584291));
#13179=CARTESIAN_POINT('',(-0.146408012399712,0.000128195943346294,0.358934495415711));
#13180=CARTESIAN_POINT('',(-0.14635,-1.79227059055215E-17,0.));
#13181=CARTESIAN_POINT('Ctrl Pts',(-0.146416087288192,0.000126442170093593,
0.366065504584291));
#13182=CARTESIAN_POINT('Ctrl Pts',(-0.146499294961499,0.00925816812376314,
0.365568242605721));
#13183=CARTESIAN_POINT('Ctrl Pts',(-0.145718277739785,0.0183757049974218,
0.365070980627151));
#13184=CARTESIAN_POINT('Ctrl Pts',(-0.144021710151773,0.0273195705351122,
0.364573718648581));
#13185=CARTESIAN_POINT('Ctrl Pts',(-0.134992913071845,0.0749170536065741,
0.361927388769479));
#13186=CARTESIAN_POINT('Ctrl Pts',(-0.100034284522917,0.117595890322328,
0.359281058890377));
#13187=CARTESIAN_POINT('Ctrl Pts',(-0.0551469387876206,0.135821305661589,
0.356634729011275));
#13188=CARTESIAN_POINT('Ctrl Pts',(-0.0102595930523245,0.15404672100085,
0.353988399132173));
#13189=CARTESIAN_POINT('Ctrl Pts',(0.0445564698693406,0.147818714963618,
0.351342069253072));
#13190=CARTESIAN_POINT('Ctrl Pts',(0.0842110755700531,0.119987943896873,
0.34869573937397));
#13191=CARTESIAN_POINT('Ctrl Pts',(0.123865681270766,0.0921571728301272,
0.346049409494868));
#13192=CARTESIAN_POINT('Ctrl Pts',(0.148358829750526,0.0427236367338667,
0.343403079615766));
#13193=CARTESIAN_POINT('Ctrl Pts',(0.146479621605269,-0.00568615719458776,
0.340756749736664));
#13194=CARTESIAN_POINT('Ctrl Pts',(0.144600413460012,-0.0540959511230416,
0.338110419857562));
#13195=CARTESIAN_POINT('Ctrl Pts',(0.116348848689739,-0.101482002883689,
0.33546408997846));
#13196=CARTESIAN_POINT('Ctrl Pts',(0.0746561129649502,-0.126154971072205,
0.332817760099358));
#13197=CARTESIAN_POINT('Ctrl Pts',(0.0329633772401616,-0.150827939260721,
0.330171430220256));
#13198=CARTESIAN_POINT('Ctrl Pts',(-0.0221705294391424,-0.152787823877104,
0.327525100341154));
#13199=CARTESIAN_POINT('Ctrl Pts',(-0.0655099505772086,-0.131137554898038,
0.324878770462052));
#13200=CARTESIAN_POINT('Ctrl Pts',(-0.108849371715275,-0.109487285918972,
0.322232440582951));
#13201=CARTESIAN_POINT('Ctrl Pts',(-0.140394307312104,-0.0642268633444555,
0.319586110703849));
#13202=CARTESIAN_POINT('Ctrl Pts',(-0.14570614405606,-0.0160726946583056,
0.316939780824747));
#13203=CARTESIAN_POINT('Ctrl Pts',(-0.146291106736525,-0.0107697471190636,
0.316648355411261));
#13204=CARTESIAN_POINT('Ctrl Pts',(-0.146557930734812,-0.0054317060295066,
0.316356929997776));
#13205=CARTESIAN_POINT('Ctrl Pts',(-0.146519404976022,-8.97763884284003E-5,
0.316065504584291));
#13206=CARTESIAN_POINT('Ctrl Pts',(-0.146528765763263,-8.45393868379275E-5,
0.30893449541571));
#13207=CARTESIAN_POINT('Ctrl Pts',(-0.146562807199252,-0.00503327764821679,
0.30920451587328));
#13208=CARTESIAN_POINT('Ctrl Pts',(-0.14633385314783,-0.00997882882536714,
0.30947453633085));
#13209=CARTESIAN_POINT('Ctrl Pts',(-0.145831525524598,-0.0148964553326841,
0.309744556788419));
#13210=CARTESIAN_POINT('Ctrl Pts',(-0.140906503086998,-0.0631108472318147,
0.312391946162679));
#13211=CARTESIAN_POINT('Ctrl Pts',(-0.109703085900295,-0.108640943453547,
0.31503933553694));
#13212=CARTESIAN_POINT('Ctrl Pts',(-0.0665140418604196,-0.13063162118607,
0.3176867249112));
#13213=CARTESIAN_POINT('Ctrl Pts',(-0.0233249978205455,-0.152622298918592,
0.32033411428546));
#13214=CARTESIAN_POINT('Ctrl Pts',(0.0318496730725009,-0.151073558161906,
0.322981503659719));
#13215=CARTESIAN_POINT('Ctrl Pts',(0.0737371373950496,-0.126694801736668,
0.325628893033979));
#13216=CARTESIAN_POINT('Ctrl Pts',(0.115624601717599,-0.10231604531143,
0.328276282408239));
#13217=CARTESIAN_POINT('Ctrl Pts',(0.144224859469651,-0.0551072732176397,
0.3309236717825));
#13218=CARTESIAN_POINT('Ctrl Pts',(0.146437523492708,-0.0066925280449658,
0.33357106115676));
#13219=CARTESIAN_POINT('Ctrl Pts',(0.148650187515766,0.0417222171277085,
0.33621845053102));
#13220=CARTESIAN_POINT('Ctrl Pts',(0.124475257809829,0.0913429353792657,
0.33886583990528));
#13221=CARTESIAN_POINT('Ctrl Pts',(0.0849860939726622,0.119440788885456,
0.34151322927954));
#13222=CARTESIAN_POINT('Ctrl Pts',(0.0454969301354961,0.147538642391646,
0.344160618653799));
#13223=CARTESIAN_POINT('Ctrl Pts',(-0.00930646783289898,0.154113631152469,
0.346808008028059));
#13224=CARTESIAN_POINT('Ctrl Pts',(-0.0543213285795041,0.136154072578339,
0.349455397402319));
#13225=CARTESIAN_POINT('Ctrl Pts',(-0.0993361893261098,0.11819451400421,
0.352102786776579));
#13226=CARTESIAN_POINT('Ctrl Pts',(-0.134562512850926,0.0757004080951257,
0.35475017615084));
#13227=CARTESIAN_POINT('Ctrl Pts',(-0.143864833510727,0.0281362381501331,
0.3573975655251));
#13228=CARTESIAN_POINT('Ctrl Pts',(-0.145664973529558,0.0189318504589563,
0.357909875488637));
#13229=CARTESIAN_POINT('Ctrl Pts',(-0.146494308508217,0.00953759842677947,
0.358422185452174));
#13230=CARTESIAN_POINT('Ctrl Pts',(-0.146408012399712,0.000128195943346294,
0.358934495415711));
#13231=CARTESIAN_POINT('Origin',(0.,0.,0.));
#13232=CARTESIAN_POINT('',(-0.146110491840834,1.12683595067248E-5,0.416065504584291));
#13233=CARTESIAN_POINT('',(-0.146109756335714,8.81622270207575E-6,0.40893449541571));
#13234=CARTESIAN_POINT('',(-0.14635,-1.79227059055215E-17,0.));
#13235=CARTESIAN_POINT('Ctrl Pts',(-0.146110491840834,1.12683595067248E-5,
0.416065504584291));
#13236=CARTESIAN_POINT('Ctrl Pts',(-0.146126798292857,0.0237518011834032,
0.414779555213666));
#13237=CARTESIAN_POINT('Ctrl Pts',(-0.140669750958991,0.0474852665485293,
0.413493605843041));
#13238=CARTESIAN_POINT('Ctrl Pts',(-0.129698698951591,0.0683144158983218,
0.412207656472415));
#13239=CARTESIAN_POINT('Ctrl Pts',(-0.107121587134001,0.111178312051432,
0.409561326593314));
#13240=CARTESIAN_POINT('Ctrl Pts',(-0.0611933749717542,0.141742803557285,
0.406914996714211));
#13241=CARTESIAN_POINT('Ctrl Pts',(-0.0129361277491455,0.146018041789781,
0.40426866683511));
#13242=CARTESIAN_POINT('Ctrl Pts',(0.0353211194734639,0.150293280022276,
0.401622336956008));
#13243=CARTESIAN_POINT('Ctrl Pts',(0.0859074017564354,0.128279264981412,
0.398976007076906));
#13244=CARTESIAN_POINT('Ctrl Pts',(0.115668581836909,0.0900521576926538,
0.396329677197804));
#13245=CARTESIAN_POINT('Ctrl Pts',(0.145429761917382,0.0518250504038959,
0.393683347318702));
#13246=CARTESIAN_POINT('Ctrl Pts',(0.154365839795359,-0.0026151491327561,
0.3910370174396));
#13247=CARTESIAN_POINT('Ctrl Pts',(0.138386632036901,-0.0483503050946702,
0.388390687560498));
#13248=CARTESIAN_POINT('Ctrl Pts',(0.122407424278443,-0.094085461056585,
0.385744357681396));
#13249=CARTESIAN_POINT('Ctrl Pts',(0.0815129308835505,-0.131115573443762,
0.383098027802294));
#13250=CARTESIAN_POINT('Ctrl Pts',(0.0344212048624006,-0.142491377230642,
0.380451697923192));
#13251=CARTESIAN_POINT('Ctrl Pts',(-0.0126705211587486,-0.153867181017521,
0.37780536804409));
#13252=CARTESIAN_POINT('Ctrl Pts',(-0.0659594798061549,-0.139588676204105,
0.375159038164988));
#13253=CARTESIAN_POINT('Ctrl Pts',(-0.101054476324393,-0.106191359083811,
0.372512708285887));
#13254=CARTESIAN_POINT('Ctrl Pts',(-0.129554902927378,-0.0790696072742943,
0.370363640385355));
#13255=CARTESIAN_POINT('Ctrl Pts',(-0.146056480184715,-0.0393390709180539,
0.368214572484823));
#13256=CARTESIAN_POINT('Ctrl Pts',(-0.146416087288192,0.000126442170093593,
0.366065504584291));
#13257=CARTESIAN_POINT('Ctrl Pts',(-0.146408012399712,0.000128195943346294,
0.358934495415711));
#13258=CARTESIAN_POINT('Ctrl Pts',(-0.146048368712081,-0.0390859965171687,
0.361069574826434));
#13259=CARTESIAN_POINT('Ctrl Pts',(-0.1297855810823,-0.0785633296797545,
0.363204654237157));
#13260=CARTESIAN_POINT('Ctrl Pts',(-0.101613371150224,-0.105657280969165,
0.36533973364788));
#13261=CARTESIAN_POINT('Ctrl Pts',(-0.066681270335132,-0.139252396162569,
0.36798712302214));
#13262=CARTESIAN_POINT('Ctrl Pts',(-0.0134387509101597,-0.153808392568477,
0.370634512396399));
#13263=CARTESIAN_POINT('Ctrl Pts',(0.0337263783221333,-0.142657876135818,
0.373281901770659));
#13264=CARTESIAN_POINT('Ctrl Pts',(0.0808915075544263,-0.13150735970316,
0.375929291144919));
#13265=CARTESIAN_POINT('Ctrl Pts',(0.12197924659404,-0.0946503304319347,
0.378576680519179));
#13266=CARTESIAN_POINT('Ctrl Pts',(0.138169300408926,-0.0489692009616054,
0.38122406989344));
#13267=CARTESIAN_POINT('Ctrl Pts',(0.154359354223812,-0.00328807149127619,
0.3838714592677));
#13268=CARTESIAN_POINT('Ctrl Pts',(0.14565172281397,0.0512171581781573,
0.38651884864196));
#13269=CARTESIAN_POINT('Ctrl Pts',(0.11603494864959,0.0895802930905963,
0.38916623801622));
#13270=CARTESIAN_POINT('Ctrl Pts',(0.0864181744852101,0.127943428003035,
0.39181362739048));
#13271=CARTESIAN_POINT('Ctrl Pts',(0.0358922575662923,0.15016446815848,
0.394461016764739));
#13272=CARTESIAN_POINT('Ctrl Pts',(-0.0123993367959677,0.146065035738641,
0.397108406138999));
#13273=CARTESIAN_POINT('Ctrl Pts',(-0.0606909311582276,0.141965603318802,
0.399755795513259));
#13274=CARTESIAN_POINT('Ctrl Pts',(-0.106748202963829,0.111545698323679,
0.40240318488752));
#13275=CARTESIAN_POINT('Ctrl Pts',(-0.129474555904152,0.0687391998188283,
0.40505057426178));
#13276=CARTESIAN_POINT('Ctrl Pts',(-0.140588317483115,0.0478057390183907,
0.406345214646423));
#13277=CARTESIAN_POINT('Ctrl Pts',(-0.146122589096428,0.0239100770892618,
0.407639855031067));
#13278=CARTESIAN_POINT('Ctrl Pts',(-0.146109756335714,8.81622270207575E-6,
0.40893449541571));
#13279=CARTESIAN_POINT('Origin',(0.,0.,0.));
#13280=CARTESIAN_POINT('',(-0.146374718215768,-0.000132229735885947,0.466065504584291));
#13281=CARTESIAN_POINT('',(-0.146375609273197,-0.000132432188538665,0.458934495415711));
#13282=CARTESIAN_POINT('',(-0.14635,-1.79227059055215E-17,0.));
#13283=CARTESIAN_POINT('Ctrl Pts',(-0.146374718215768,-0.000132229735885947,
0.466065504584291));
#13284=CARTESIAN_POINT('Ctrl Pts',(-0.146022504084922,0.0379941335185874,
0.46399086782161));
#13285=CARTESIAN_POINT('Ctrl Pts',(-0.130761950520226,0.0763703265456945,
0.46191623105893));
#13286=CARTESIAN_POINT('Ctrl Pts',(-0.103994021541854,0.103314352404769,
0.45984159429625));
#13287=CARTESIAN_POINT('Ctrl Pts',(-0.0698498419286355,0.137683154682254,
0.457195264417148));
#13288=CARTESIAN_POINT('Ctrl Pts',(-0.0169824611430249,0.153451124186949,
0.454548934538046));
#13289=CARTESIAN_POINT('Ctrl Pts',(0.030409888879481,0.143401013202843,
0.451902604658944));
#13290=CARTESIAN_POINT('Ctrl Pts',(0.0778022389019875,0.133350902218736,
0.449256274779842));
#13291=CARTESIAN_POINT('Ctrl Pts',(0.119719558161389,0.0974827107458278,
0.44660994490074));
#13292=CARTESIAN_POINT('Ctrl Pts',(0.136975630157447,0.0522138743269898,
0.443963615021638));
#13293=CARTESIAN_POINT('Ctrl Pts',(0.154231702153504,0.00694503790815254,
0.441317285142536));
#13294=CARTESIAN_POINT('Ctrl Pts',(0.146826526886218,-0.0477244434566137,
0.438670955263434));
#13295=CARTESIAN_POINT('Ctrl Pts',(0.118149569579287,-0.0867714880447125,
0.436024625384332));
#13296=CARTESIAN_POINT('Ctrl Pts',(0.0894726122723542,-0.125818532632812,
0.43337829550523));
#13297=CARTESIAN_POINT('Ctrl Pts',(0.0395238729257754,-0.149243140444243,
0.430731965626129));
#13298=CARTESIAN_POINT('Ctrl Pts',(-0.00883432462988853,-0.146323499949933,
0.428085635747027));
#13299=CARTESIAN_POINT('Ctrl Pts',(-0.0571925221855517,-0.143403859455623,
0.425439305867925));
#13300=CARTESIAN_POINT('Ctrl Pts',(-0.1039601779503,-0.114139970655572,
0.422792975988823));
#13301=CARTESIAN_POINT('Ctrl Pts',(-0.127731000096207,-0.0719263758553634,
0.420146646109721));
#13302=CARTESIAN_POINT('Ctrl Pts',(-0.139950702323481,-0.0502259249733931,
0.418786265601244));
#13303=CARTESIAN_POINT('Ctrl Pts',(-0.146093241566443,-0.0251033736724598,
0.417425885092767));
#13304=CARTESIAN_POINT('Ctrl Pts',(-0.146110491840834,1.12683595067248E-5,
0.416065504584291));
#13305=CARTESIAN_POINT('Ctrl Pts',(-0.146109756335714,8.81622270207575E-6,
0.40893449541571));
#13306=CARTESIAN_POINT('Ctrl Pts',(-0.146096347589706,-0.0249652282079418,
0.410287244405327));
#13307=CARTESIAN_POINT('Ctrl Pts',(-0.140026707259891,-0.049945385460595,
0.411639993394943));
#13308=CARTESIAN_POINT('Ctrl Pts',(-0.127937780377622,-0.0715588049813403,
0.412992742384559));
#13309=CARTESIAN_POINT('Ctrl Pts',(-0.104279217835726,-0.113857219262079,
0.415640131758819));
#13310=CARTESIAN_POINT('Ctrl Pts',(-0.0575666586768896,-0.14326095580898,
0.41828752113308));
#13311=CARTESIAN_POINT('Ctrl Pts',(-0.00919685447762893,-0.146301592903247,
0.42093491050734));
#13312=CARTESIAN_POINT('Ctrl Pts',(0.039172949721632,-0.149342229997515,
0.4235822998816));
#13313=CARTESIAN_POINT('Ctrl Pts',(0.089199998961318,-0.126019767639148,
0.426229689255859));
#13314=CARTESIAN_POINT('Ctrl Pts',(0.117969334952632,-0.0870170915920772,
0.428877078630119));
#13315=CARTESIAN_POINT('Ctrl Pts',(0.146738670943946,-0.0480144155450057,
0.431524468004379));
#13316=CARTESIAN_POINT('Ctrl Pts',(0.154250293686888,0.00666847419077017,
0.43417185737864));
#13317=CARTESIAN_POINT('Ctrl Pts',(0.137063494116028,0.051984005222912,
0.4368192467529));
#13318=CARTESIAN_POINT('Ctrl Pts',(0.119876694545168,0.0972995362550541,
0.43946663612716));
#13319=CARTESIAN_POINT('Ctrl Pts',(0.0779914726605056,0.133247708583562,
0.442114025501419));
#13320=CARTESIAN_POINT('Ctrl Pts',(0.0305934116013849,0.143362412733947,
0.444761414875679));
#13321=CARTESIAN_POINT('Ctrl Pts',(-0.0168046494577345,0.153477116884331,
0.447408804249939));
#13322=CARTESIAN_POINT('Ctrl Pts',(-0.0697155496913122,0.137758352856595,
0.4500561936242));
#13323=CARTESIAN_POINT('Ctrl Pts',(-0.103903378920715,0.103406122000434,
0.45270358299846));
#13324=CARTESIAN_POINT('Ctrl Pts',(-0.130724942802416,0.0764555792150183,
0.45478055380421));
#13325=CARTESIAN_POINT('Ctrl Pts',(-0.146022533856355,0.0380362146017157,
0.45685752460996));
#13326=CARTESIAN_POINT('Ctrl Pts',(-0.146375609273197,-0.000132432188538665,
0.458934495415711));
#13327=CARTESIAN_POINT('Origin',(0.,0.,0.));
#13328=CARTESIAN_POINT('',(-0.146548608312775,6.99729089778146E-5,0.516065504584291));
#13329=CARTESIAN_POINT('',(-0.146550766805835,6.86360251013434E-5,0.508934495415711));
#13330=CARTESIAN_POINT('',(-0.14635,-1.79227059055215E-17,0.));
#13331=CARTESIAN_POINT('Ctrl Pts',(-0.146548608312775,6.99729089778146E-5,
0.516065504584291));
#13332=CARTESIAN_POINT('Ctrl Pts',(-0.146572081366671,0.00404546554386884,
0.515848510308657));
#13333=CARTESIAN_POINT('Ctrl Pts',(-0.146424333269732,0.00801918670503405,
0.515631516033023));
#13334=CARTESIAN_POINT('Ctrl Pts',(-0.146099725131082,0.0119784074854107,
0.51541452175739));
#13335=CARTESIAN_POINT('Ctrl Pts',(-0.142141002193345,0.06026265009261,
0.512768191878288));
#13336=CARTESIAN_POINT('Ctrl Pts',(-0.111878319621163,0.106390286678145,
0.510121861999186));
#13337=CARTESIAN_POINT('Ctrl Pts',(-0.069163383343408,0.129247972261684,
0.507475532120084));
#13338=CARTESIAN_POINT('Ctrl Pts',(-0.0264484470656534,0.152105657845224,
0.504829202240982));
#13339=CARTESIAN_POINT('Ctrl Pts',(0.0287187429176733,0.151693392426768,
0.50218287236188));
#13340=CARTESIAN_POINT('Ctrl Pts',(0.07108729581893,0.128199876374419,0.499536542482778));
#13341=CARTESIAN_POINT('Ctrl Pts',(0.113455848720186,0.10470636032207,0.496890212603677));
#13342=CARTESIAN_POINT('Ctrl Pts',(0.143025764539373,0.0581315936358261,
0.494243882724575));
#13343=CARTESIAN_POINT('Ctrl Pts',(0.146262427589597,0.00979357977770552,
0.491597552845473));
#13344=CARTESIAN_POINT('Ctrl Pts',(0.149499090639821,-0.0385444340804161,
0.488951222966371));
#13345=CARTESIAN_POINT('Ctrl Pts',(0.126402500921083,-0.0886456951104151,
0.486304893087269));
#13346=CARTESIAN_POINT('Ctrl Pts',(0.087544330920799,-0.117578067907642,
0.483658563208167));
#13347=CARTESIAN_POINT('Ctrl Pts',(0.0486861609205161,-0.146510440704867,
0.481012233329065));
#13348=CARTESIAN_POINT('Ctrl Pts',(-0.00593358936131212,-0.154273925269321,
0.478365903449963));
#13349=CARTESIAN_POINT('Ctrl Pts',(-0.0513146009011563,-0.137315052574797,
0.475719573570861));
#13350=CARTESIAN_POINT('Ctrl Pts',(-0.0966956124410008,-0.120356179880273,
0.473073243691759));
#13351=CARTESIAN_POINT('Ctrl Pts',(-0.132837885238862,-0.078674949926771,
0.470426913812657));
#13352=CARTESIAN_POINT('Ctrl Pts',(-0.14319853241738,-0.0313495174248821,
0.467780583933555));
#13353=CARTESIAN_POINT('Ctrl Pts',(-0.145436768368387,-0.0211256884885646,
0.467208890817134));
#13354=CARTESIAN_POINT('Ctrl Pts',(-0.146471775395962,-0.0106384445195334,
0.466637197700712));
#13355=CARTESIAN_POINT('Ctrl Pts',(-0.146374718215768,-0.000132229735885947,
0.466065504584291));
#13356=CARTESIAN_POINT('Ctrl Pts',(-0.146375609273197,-0.000132432188538665,
0.458934495415711));
#13357=CARTESIAN_POINT('Ctrl Pts',(-0.146472577787773,-0.0106150565970108,
0.45950491398422));
#13358=CARTESIAN_POINT('Ctrl Pts',(-0.145442327125792,-0.021078770125739,
0.46007533255273));
#13359=CARTESIAN_POINT('Ctrl Pts',(-0.143213999951756,-0.0312807998000163,
0.460645751121239));
#13360=CARTESIAN_POINT('Ctrl Pts',(-0.132872033528166,-0.0786297930597184,
0.463293140495499));
#13361=CARTESIAN_POINT('Ctrl Pts',(-0.0967233424557573,-0.120342081894533,
0.465940529869759));
#13362=CARTESIAN_POINT('Ctrl Pts',(-0.0513258840937604,-0.13731129538499,
0.46858791924402));
#13363=CARTESIAN_POINT('Ctrl Pts',(-0.00592842573176499,-0.154280508875447,
0.47123530861828));
#13364=CARTESIAN_POINT('Ctrl Pts',(0.0487177999198187,-0.146506647021548,
0.47388269799254));
#13365=CARTESIAN_POINT('Ctrl Pts',(0.0875820145025328,-0.117550537871965,
0.476530087366799));
#13366=CARTESIAN_POINT('Ctrl Pts',(0.126446229085248,-0.0885944287223814,
0.47917747674106));
#13367=CARTESIAN_POINT('Ctrl Pts',(0.149528432599094,-0.0384560722771122,
0.481824866115319));
#13368=CARTESIAN_POINT('Ctrl Pts',(0.146255790172295,0.0098985887573764,
0.484472255489579));
#13369=CARTESIAN_POINT('Ctrl Pts',(0.142983147745498,0.0582532497918637,
0.487119644863839));
#13370=CARTESIAN_POINT('Ctrl Pts',(0.113355659378058,0.10482421541557,0.4897670342381));
#13371=CARTESIAN_POINT('Ctrl Pts',(0.0709442366160257,0.128279591164298,
0.49241442361236));
#13372=CARTESIAN_POINT('Ctrl Pts',(0.0285328138539934,0.151734966913027,
0.49506181298662));
#13373=CARTESIAN_POINT('Ctrl Pts',(-0.0266625433026316,0.152074752786777,
0.497709202360879));
#13374=CARTESIAN_POINT('Ctrl Pts',(-0.0693595260588707,0.129143309401606,
0.500356591735139));
#13375=CARTESIAN_POINT('Ctrl Pts',(-0.11205650881511,0.106211866016435,
0.503003981109399));
#13376=CARTESIAN_POINT('Ctrl Pts',(-0.142255117170964,0.060009193372344,
0.505651370483659));
#13377=CARTESIAN_POINT('Ctrl Pts',(-0.146122837288996,0.0116984888307781,
0.50829875985792));
#13378=CARTESIAN_POINT('Ctrl Pts',(-0.146432431239741,0.00783142983325791,
0.508510671710517));
#13379=CARTESIAN_POINT('Ctrl Pts',(-0.14657331536999,0.00395086404934249,
0.508722583563114));
#13380=CARTESIAN_POINT('Ctrl Pts',(-0.146550766805835,6.86360251013434E-5,
0.508934495415711));
#13381=CARTESIAN_POINT('Origin',(0.,0.,0.));
#13382=CARTESIAN_POINT('',(-0.146165204287215,8.83645032875094E-5,0.566065504584291));
#13383=CARTESIAN_POINT('',(-0.146168951232552,9.12430751481418E-5,0.558934495415711));
#13384=CARTESIAN_POINT('',(-0.14635,-1.79227059055215E-17,0.));
#13385=CARTESIAN_POINT('Ctrl Pts',(-0.146165204287215,8.83645032875094E-5,
0.566065504584291));
#13386=CARTESIAN_POINT('Ctrl Pts',(-0.146267412293664,0.0186373661349918,
0.565059822916602));
#13387=CARTESIAN_POINT('Ctrl Pts',(-0.142994166834961,0.0371516370495788,
0.564054141248913));
#13388=CARTESIAN_POINT('Ctrl Pts',(-0.136179985035193,0.0542551712289143,
0.563048459581224));
#13389=CARTESIAN_POINT('Ctrl Pts',(-0.118249288396568,0.0992610562830057,
0.560402129702122));
#13390=CARTESIAN_POINT('Ctrl Pts',(-0.0758005933416487,0.134498778989873,
0.55775579982302));
#13391=CARTESIAN_POINT('Ctrl Pts',(-0.0282633354322908,0.143839479279877,
0.555109469943918));
#13392=CARTESIAN_POINT('Ctrl Pts',(0.0192739224770691,0.153180179569881,
0.552463140064816));
#13393=CARTESIAN_POINT('Ctrl Pts',(0.0718997432408687,0.136623857443018,
0.549816810185715));
#13394=CARTESIAN_POINT('Ctrl Pts',(0.105526460745998,0.101748602013432,
0.547170480306613));
#13395=CARTESIAN_POINT('Ctrl Pts',(0.139153178251127,0.0668733465838454,
0.544524150427511));
#13396=CARTESIAN_POINT('Ctrl Pts',(0.153780792497586,0.0136791578515372,
0.541877820548409));
#13397=CARTESIAN_POINT('Ctrl Pts',(0.142714014311998,-0.0334861471092027,
0.539231490669307));
#13398=CARTESIAN_POINT('Ctrl Pts',(0.13164723612641,-0.0806514520699426,
0.536585160790205));
#13399=CARTESIAN_POINT('Ctrl Pts',(0.0948860655087725,-0.121787873259113,
0.533938830911103));
#13400=CARTESIAN_POINT('Ctrl Pts',(0.0492566686055307,-0.138066623508903,
0.531292501032001));
#13401=CARTESIAN_POINT('Ctrl Pts',(0.00362727170228945,-0.154345373758693,
0.528646171152899));
#13402=CARTESIAN_POINT('Ctrl Pts',(-0.050870351486557,-0.145766453069103,
0.525999841273797));
#13403=CARTESIAN_POINT('Ctrl Pts',(-0.089291781429334,-0.116256568409877,
0.523353511394695));
#13404=CARTESIAN_POINT('Ctrl Pts',(-0.124562723435938,-0.0891664410515947,
0.520924175791227));
#13405=CARTESIAN_POINT('Ctrl Pts',(-0.146285818313441,-0.0444372186796531,
0.518494840187759));
#13406=CARTESIAN_POINT('Ctrl Pts',(-0.146548608312775,6.99729089778146E-5,
0.516065504584291));
#13407=CARTESIAN_POINT('Ctrl Pts',(-0.146550766805835,6.86360251013434E-5,
0.508934495415711));
#13408=CARTESIAN_POINT('Ctrl Pts',(-0.146291618860727,-0.0445493453248537,
0.511369972937373));
#13409=CARTESIAN_POINT('Ctrl Pts',(-0.124445252016267,-0.0893868858389474,
0.513805450459036));
#13410=CARTESIAN_POINT('Ctrl Pts',(-0.0890226177929609,-0.116463349340462,
0.516240927980699));
#13411=CARTESIAN_POINT('Ctrl Pts',(-0.0505178462986829,-0.145895746531099,
0.518888317354959));
#13412=CARTESIAN_POINT('Ctrl Pts',(0.00402852857008221,-0.154341804473332,
0.52153570672922));
#13413=CARTESIAN_POINT('Ctrl Pts',(0.0496314652424392,-0.137932794781367,
0.52418309610348));
#13414=CARTESIAN_POINT('Ctrl Pts',(0.0952344019147948,-0.121523785089403,
0.52683048547774));
#13415=CARTESIAN_POINT('Ctrl Pts',(0.131893900390741,-0.0802597077632436,
0.529477874851999));
#13416=CARTESIAN_POINT('Ctrl Pts',(0.14281802728161,-0.0330416298281342,
0.532125264226259));
#13417=CARTESIAN_POINT('Ctrl Pts',(0.153742154172479,0.0141764481069759,
0.53477265360052));
#13418=CARTESIAN_POINT('Ctrl Pts',(0.138930909478268,0.0673485266510362,
0.53742004297478));
#13419=CARTESIAN_POINT('Ctrl Pts',(0.105168604077417,0.102119062543277,
0.54006743234904));
#13420=CARTESIAN_POINT('Ctrl Pts',(0.0714062986765666,0.136889598435517,
0.5427148217233));
#13421=CARTESIAN_POINT('Ctrl Pts',(0.018692932569077,0.153258591675938,
0.545362211097559));
#13422=CARTESIAN_POINT('Ctrl Pts',(-0.0288260648428939,0.143728202535144,
0.548009600471819));
#13423=CARTESIAN_POINT('Ctrl Pts',(-0.0763450622548654,0.13419781339435,
0.550656989846079));
#13424=CARTESIAN_POINT('Ctrl Pts',(-0.118669690971318,0.0987680418723385,
0.55330437922034));
#13425=CARTESIAN_POINT('Ctrl Pts',(-0.136413096952957,0.0536675432455532,
0.5559517685946));
#13426=CARTESIAN_POINT('Ctrl Pts',(-0.143076734904351,0.036729792140314,
0.556946010868304));
#13427=CARTESIAN_POINT('Ctrl Pts',(-0.146273385252938,0.0184280612467595,
0.557940253142007));
#13428=CARTESIAN_POINT('Ctrl Pts',(-0.146168951232552,9.12430751481418E-5,
0.558934495415711));
#13429=CARTESIAN_POINT('Origin',(0.,0.,0.));
#13430=CARTESIAN_POINT('',(-0.146227179098081,-0.000117664897458569,0.616065504584291));
#13431=CARTESIAN_POINT('',(-0.146218520919543,-0.000115076211918358,0.608934495415711));
#13432=CARTESIAN_POINT('',(-0.14635,-1.79227059055215E-17,0.));
#13433=CARTESIAN_POINT('Ctrl Pts',(-0.146227179098081,-0.000117664897458569,
0.616065504584291));
#13434=CARTESIAN_POINT('Ctrl Pts',(-0.145977603365176,0.0329427899635141,
0.614271135524546));
#13435=CARTESIAN_POINT('Ctrl Pts',(-0.134874795495675,0.0661550248562671,
0.612476766464802));
#13436=CARTESIAN_POINT('Ctrl Pts',(-0.114309815624116,0.091770790457776,
0.610682397405058));
#13437=CARTESIAN_POINT('Ctrl Pts',(-0.0839806476072558,0.129548841477563,
0.608036067525956));
#13438=CARTESIAN_POINT('Ctrl Pts',(-0.0330710111925292,0.150804375664025,
0.605389737646855));
#13439=CARTESIAN_POINT('Ctrl Pts',(0.0151169520838501,0.145808400611758,
0.602743407767753));
#13440=CARTESIAN_POINT('Ctrl Pts',(0.0633049153602295,0.140812425559491,
0.600097077888651));
#13441=CARTESIAN_POINT('Ctrl Pts',(0.108771205498262,0.109564941268491,
0.597450748009549));
#13442=CARTESIAN_POINT('Ctrl Pts',(0.130705186191441,0.0663684129079872,
0.594804418130447));
#13443=CARTESIAN_POINT('Ctrl Pts',(0.152639166884621,0.023171884547483,
0.592158088251345));
#13444=CARTESIAN_POINT('Ctrl Pts',(0.151040838132949,-0.0319736878825246,
0.589511758372243));
#13445=CARTESIAN_POINT('Ctrl Pts',(0.126641780152193,-0.0738273082886534,
0.586865428493141));
#13446=CARTESIAN_POINT('Ctrl Pts',(0.102242722171437,-0.115680928694782,
0.584219098614039));
#13447=CARTESIAN_POINT('Ctrl Pts',(0.0550429349615966,-0.14424259707703,
0.581572768734937));
#13448=CARTESIAN_POINT('Ctrl Pts',(0.00664650371163741,-0.14643918846291,
0.578926438855836));
#13449=CARTESIAN_POINT('Ctrl Pts',(-0.0417499275383225,-0.148635779848789,
0.576280108976733));
#13450=CARTESIAN_POINT('Ctrl Pts',(-0.0913430028284016,-0.1244672942383,
0.573633779097631));
#13451=CARTESIAN_POINT('Ctrl Pts',(-0.119433191362276,-0.0849960277323969,
0.570987449218529));
#13452=CARTESIAN_POINT('Ctrl Pts',(-0.136848298201485,-0.0605249807527623,
0.569346801007117));
#13453=CARTESIAN_POINT('Ctrl Pts',(-0.145998464265635,-0.0301720919893573,
0.567706152795704));
#13454=CARTESIAN_POINT('Ctrl Pts',(-0.146165204287215,8.83645032875094E-5,
0.566065504584291));
#13455=CARTESIAN_POINT('Ctrl Pts',(-0.146168951232552,9.12430751481418E-5,
0.558934495415711));
#13456=CARTESIAN_POINT('Ctrl Pts',(-0.145995306636495,-0.0303977620653178,
0.560587642516267));
#13457=CARTESIAN_POINT('Ctrl Pts',(-0.136695352934655,-0.0609837708898569,
0.562240789616823));
#13458=CARTESIAN_POINT('Ctrl Pts',(-0.119031718004195,-0.0855580991331628,
0.563893936717379));
#13459=CARTESIAN_POINT('Ctrl Pts',(-0.090744749826965,-0.124912017153538,
0.566541326091639));
#13460=CARTESIAN_POINT('Ctrl Pts',(-0.0410086302256792,-0.148848627462727,
0.5691887154659));
#13461=CARTESIAN_POINT('Ctrl Pts',(0.00739494322942312,-0.146403732988417,
0.57183610484016));
#13462=CARTESIAN_POINT('Ctrl Pts',(0.0557985166845234,-0.143958838514108,
0.57448349421442));
#13463=CARTESIAN_POINT('Ctrl Pts',(0.10286954399344,-0.1151324392563,0.57713088358868));
#13464=CARTESIAN_POINT('Ctrl Pts',(0.127047076753504,-0.0731285067993286,
0.579778272962939));
#13465=CARTESIAN_POINT('Ctrl Pts',(0.151224609513568,-0.031124574342357,
0.5824256623372));
#13466=CARTESIAN_POINT('Ctrl Pts',(0.15250864772478,0.0240568913137802,
0.58507305171146));
#13467=CARTESIAN_POINT('Ctrl Pts',(0.130311035929276,0.0671399443948921,
0.58772044108572));
#13468=CARTESIAN_POINT('Ctrl Pts',(0.108113424133771,0.110222997476006,
0.59036783045998));
#13469=CARTESIAN_POINT('Ctrl Pts',(0.0624341623315493,0.141207637982093,
0.593015219834239));
#13470=CARTESIAN_POINT('Ctrl Pts',(0.0141966988324609,0.145901308974836,
0.595662609208499));
#13471=CARTESIAN_POINT('Ctrl Pts',(-0.0340407646666261,0.150594979967579,
0.598309998582759));
#13472=CARTESIAN_POINT('Ctrl Pts',(-0.0848364298625779,0.128997681446978,
0.60095738795702));
#13473=CARTESIAN_POINT('Ctrl Pts',(-0.114923272877171,0.091002085522857,
0.60360477733128));
#13474=CARTESIAN_POINT('Ctrl Pts',(-0.135113526827902,0.0655045372973676,
0.60538135002609));
#13475=CARTESIAN_POINT('Ctrl Pts',(-0.14597798884013,0.0326223532682757,
0.6071579227209));
#13476=CARTESIAN_POINT('Ctrl Pts',(-0.146218520919543,-0.000115076211918358,
0.608934495415711));
#13477=CARTESIAN_POINT('Origin',(0.,0.,0.));
#13478=CARTESIAN_POINT('',(-0.146586033401767,-2.15382961294558E-5,0.66606550458429));
#13479=CARTESIAN_POINT('',(-0.146582846697157,-3.00215943766004E-5,0.65893449541571));
#13480=CARTESIAN_POINT('',(-0.14635,-1.79227059055215E-17,0.));
#13481=CARTESIAN_POINT('Ctrl Pts',(-0.146586033401767,-2.15382961294558E-5,
0.66606550458429));
#13482=CARTESIAN_POINT('Ctrl Pts',(-0.146488810225965,0.0472697707580183,
0.663482448132491));
#13483=CARTESIAN_POINT('Ctrl Pts',(-0.121516563758978,0.0946492637554097,
0.660899391680692));
#13484=CARTESIAN_POINT('Ctrl Pts',(-0.0824084263440199,0.121233094478226,
0.658316335228893));
#13485=CARTESIAN_POINT('Ctrl Pts',(-0.0423423130056393,0.148468111155377,
0.655670005349791));
#13486=CARTESIAN_POINT('Ctrl Pts',(0.0125607065496858,0.153876184485078,
0.653023675470689));
#13487=CARTESIAN_POINT('Ctrl Pts',(0.0571706564953393,0.134981954220393,
0.650377345591587));
#13488=CARTESIAN_POINT('Ctrl Pts',(0.101780606440992,0.116087723955709,
0.647731015712485));
#13489=CARTESIAN_POINT('Ctrl Pts',(0.136097486776972,0.0728911900966409,
0.645084685833384));
#13490=CARTESIAN_POINT('Ctrl Pts',(0.144413921474191,0.0251640857912735,
0.642438355954282));
#13491=CARTESIAN_POINT('Ctrl Pts',(0.152730356171409,-0.0225630185140953,
0.63979202607518));
#13492=CARTESIAN_POINT('Ctrl Pts',(0.135046345229863,-0.0748206932657649,
0.637145696196077));
#13493=CARTESIAN_POINT('Ctrl Pts',(0.0994561386758346,-0.10768977857233,
0.634499366316975));
#13494=CARTESIAN_POINT('Ctrl Pts',(0.0638659321218069,-0.140558863878895,
0.631853036437873));
#13495=CARTESIAN_POINT('Ctrl Pts',(0.0103695299552984,-0.154039359740357,
0.629206706558772));
#13496=CARTESIAN_POINT('Ctrl Pts',(-0.0365469229059137,-0.141961031115491,
0.62656037667967));
#13497=CARTESIAN_POINT('Ctrl Pts',(-0.0834633757671259,-0.129882702490626,
0.623914046800568));
#13498=CARTESIAN_POINT('Ctrl Pts',(-0.123799879323041,-0.0922455493794331,
0.621267716921466));
#13499=CARTESIAN_POINT('Ctrl Pts',(-0.139093781291504,-0.0462766888972804,
0.618621387042364));
#13500=CARTESIAN_POINT('Ctrl Pts',(-0.14401750805555,-0.0314774500153124,
0.617769426223006));
#13501=CARTESIAN_POINT('Ctrl Pts',(-0.14634567687575,-0.0158146654998378,
0.616917465403648));
#13502=CARTESIAN_POINT('Ctrl Pts',(-0.146227179098081,-0.000117664897458569,
0.616065504584291));
#13503=CARTESIAN_POINT('Ctrl Pts',(-0.146218520919543,-0.000115076211918358,
0.608934495415711));
#13504=CARTESIAN_POINT('Ctrl Pts',(-0.1463364217222,-0.0161618722236638,
0.60980531209516));
#13505=CARTESIAN_POINT('Ctrl Pts',(-0.143901781624712,-0.032173889023867,
0.61067612877461));
#13506=CARTESIAN_POINT('Ctrl Pts',(-0.138761720114909,-0.0472643972675185,
0.611546945454059));
#13507=CARTESIAN_POINT('Ctrl Pts',(-0.123135303504819,-0.0931413908061287,
0.614194334828319));
#13508=CARTESIAN_POINT('Ctrl Pts',(-0.0825044494514074,-0.130501484555709,
0.616841724202579));
#13509=CARTESIAN_POINT('Ctrl Pts',(-0.0354801761942514,-0.142231836504824,
0.619489113576839));
#13510=CARTESIAN_POINT('Ctrl Pts',(0.0115440970629072,-0.15396218845394,
0.6221365029511));
#13511=CARTESIAN_POINT('Ctrl Pts',(0.0649617895238099,-0.140062798602586,
0.624783892325359));
#13512=CARTESIAN_POINT('Ctrl Pts',(0.100304854137336,-0.106900301471969,
0.627431281699619));
#13513=CARTESIAN_POINT('Ctrl Pts',(0.135647918750861,-0.0737378043413545,
0.630078671073879));
#13514=CARTESIAN_POINT('Ctrl Pts',(0.15291635551701,-0.0213121999314781,
0.63272606044814));
#13515=CARTESIAN_POINT('Ctrl Pts',(0.144200333369931,0.026362891994447,
0.6353734498224));
#13516=CARTESIAN_POINT('Ctrl Pts',(0.135484311222852,0.0740379839203748,
0.63802083919666));
#13517=CARTESIAN_POINT('Ctrl Pts',(0.100783830162543,0.11696256336235,0.640668228570919));
#13518=CARTESIAN_POINT('Ctrl Pts',(0.055993492972559,0.135474968031154,
0.643315617945179));
#13519=CARTESIAN_POINT('Ctrl Pts',(0.0112031557825773,0.153987372699956,
0.64596300731944));
#13520=CARTESIAN_POINT('Ctrl Pts',(-0.04367703753708,0.148087602595587,
0.6486103966937));
#13521=CARTESIAN_POINT('Ctrl Pts',(-0.0835091394177698,0.120478055479053,
0.65125778606796));
#13522=CARTESIAN_POINT('Ctrl Pts',(-0.122009894390588,0.0937913289882395,
0.653816689183877));
#13523=CARTESIAN_POINT('Ctrl Pts',(-0.146451680634158,0.0468218259492564,
0.656375592299793));
#13524=CARTESIAN_POINT('Ctrl Pts',(-0.146582846697157,-3.00215943766004E-5,
0.65893449541571));
#13525=CARTESIAN_POINT('Origin',(0.,0.,0.));
#13526=CARTESIAN_POINT('',(-0.146290249280603,0.000131112932912382,0.716065504584291));
#13527=CARTESIAN_POINT('',(-0.146307221518699,0.000133045872591754,0.708934495415711));
#13528=CARTESIAN_POINT('',(-0.14635,-1.79227059055215E-17,0.));
#13529=CARTESIAN_POINT('Ctrl Pts',(-0.146290249280603,0.000131112932912382,
0.716065504584291));
#13530=CARTESIAN_POINT('Ctrl Pts',(-0.146406294125046,0.0134819654399978,
0.715340090619538));
#13531=CARTESIAN_POINT('Ctrl Pts',(-0.144729088574721,0.0268041890186768,
0.714614676654786));
#13532=CARTESIAN_POINT('Ctrl Pts',(-0.141142411757643,0.0395908011096033,
0.713889262690033));
#13533=CARTESIAN_POINT('Ctrl Pts',(-0.128058117149462,0.0862367098911347,
0.711242932810931));
#13534=CARTESIAN_POINT('Ctrl Pts',(-0.0895623832093418,0.125754646095387,
0.708596602931829));
#13535=CARTESIAN_POINT('Ctrl Pts',(-0.0432753130058998,0.140056628595385,
0.705950273052727));
#13536=CARTESIAN_POINT('Ctrl Pts',(0.00301175719754219,0.154358611095384,
0.703303943173625));
#13537=CARTESIAN_POINT('Ctrl Pts',(0.0570901636643063,0.143444639891129,
0.700657613294523));
#13538=CARTESIAN_POINT('Ctrl Pts',(0.0942073689518517,0.11231021130972,
0.698011283415421));
#13539=CARTESIAN_POINT('Ctrl Pts',(0.131324574239397,0.0811757827283121,
0.695364953536319));
#13540=CARTESIAN_POINT('Ctrl Pts',(0.151480578347723,0.0298208967697505,
0.692718623657217));
#13541=CARTESIAN_POINT('Ctrl Pts',(0.145449661086834,-0.0182485073085286,
0.690072293778115));
#13542=CARTESIAN_POINT('Ctrl Pts',(0.139418743825945,-0.0663179113868083,
0.687425963899014));
#13543=CARTESIAN_POINT('Ctrl Pts',(0.107200905195838,-0.111101833584806,
0.684779634019911));
#13544=CARTESIAN_POINT('Ctrl Pts',(0.0635427568131047,-0.132101968137704,
0.68213330414081));
#13545=CARTESIAN_POINT('Ctrl Pts',(0.0198846084303716,-0.153102102690602,
0.679486974261708));
#13546=CARTESIAN_POINT('Ctrl Pts',(-0.0352138497049885,-0.150318449598402,
0.676840644382606));
#13547=CARTESIAN_POINT('Ctrl Pts',(-0.0765331864534889,-0.125025130675956,
0.674194314503504));
#13548=CARTESIAN_POINT('Ctrl Pts',(-0.117852523201989,-0.0997318117535095,
0.671547984624402));
#13549=CARTESIAN_POINT('Ctrl Pts',(-0.14539273856363,-0.0519288270008166,
0.6689016547453));
#13550=CARTESIAN_POINT('Ctrl Pts',(-0.146548242683733,-0.00349635461217019,
0.666255324866198));
#13551=CARTESIAN_POINT('Ctrl Pts',(-0.146575870647472,-0.00233834005587287,
0.666192051438896));
#13552=CARTESIAN_POINT('Ctrl Pts',(-0.146588414938392,-0.00117996563262623,
0.666128778011593));
#13553=CARTESIAN_POINT('Ctrl Pts',(-0.146586033401767,-2.15382961294558E-5,
0.66606550458429));
#13554=CARTESIAN_POINT('Ctrl Pts',(-0.146582846697157,-3.00215943766004E-5,
0.65893449541571));
#13555=CARTESIAN_POINT('Ctrl Pts',(-0.146587382388275,-0.00165014728799839,
0.659022981674053));
#13556=CARTESIAN_POINT('Ctrl Pts',(-0.146562848415234,-0.00327013229389975,
0.659111467932396));
#13557=CARTESIAN_POINT('Ctrl Pts',(-0.146508820881567,-0.00488913307276392,
0.659199954190739));
#13558=CARTESIAN_POINT('Ctrl Pts',(-0.144892390022949,-0.0533274503793473,
0.661847343564999));
#13559=CARTESIAN_POINT('Ctrl Pts',(-0.116875517863988,-0.100884760863813,
0.66449473293926));
#13560=CARTESIAN_POINT('Ctrl Pts',(-0.0752913709948059,-0.125777373450206,
0.66714212231352));
#13561=CARTESIAN_POINT('Ctrl Pts',(-0.0337072241256252,-0.150669986036599,
0.66978951168778));
#13562=CARTESIAN_POINT('Ctrl Pts',(0.021444197453776,-0.15289790072492,
0.672436901062039));
#13563=CARTESIAN_POINT('Ctrl Pts',(0.0649007096996251,-0.131440618146733,
0.675084290436299));
#13564=CARTESIAN_POINT('Ctrl Pts',(0.108357221945475,-0.109983335568545,
0.677731679810559));
#13565=CARTESIAN_POINT('Ctrl Pts',(0.140118824857774,-0.0648408557238465,
0.68037906918482));
#13566=CARTESIAN_POINT('Ctrl Pts',(0.145637072805965,-0.0166907532130915,
0.68302645855908));
#13567=CARTESIAN_POINT('Ctrl Pts',(0.151155320754156,0.031459349297663,
0.68567384793334));
#13568=CARTESIAN_POINT('Ctrl Pts',(0.130430213738242,0.0826170744744734,
0.688321237307599));
#13569=CARTESIAN_POINT('Ctrl Pts',(0.0929549153570804,0.113349556369966,
0.690968626681859));
#13570=CARTESIAN_POINT('Ctrl Pts',(0.0554796169759186,0.14408203826546,
0.693616016056119));
#13571=CARTESIAN_POINT('Ctrl Pts',(0.00125412722950909,0.154389276879634,
0.69626340543038));
#13572=CARTESIAN_POINT('Ctrl Pts',(-0.0448834941801804,0.139550027475769,
0.69891079480464));
#13573=CARTESIAN_POINT('Ctrl Pts',(-0.0910211155898686,0.124710778071904,
0.7015581841789));
#13574=CARTESIAN_POINT('Ctrl Pts',(-0.129070868662838,0.0847250406500019,
0.704205573553159));
#13575=CARTESIAN_POINT('Ctrl Pts',(-0.141604011991841,0.0379083368947344,
0.706852962927419));
#13576=CARTESIAN_POINT('Ctrl Pts',(-0.144888775625201,0.0256383259412015,
0.707546807090183));
#13577=CARTESIAN_POINT('Ctrl Pts',(-0.146420824649375,0.0128991016161637,
0.708240651252947));
#13578=CARTESIAN_POINT('Ctrl Pts',(-0.146307221518699,0.000133045872591754,
0.708934495415711));
#13579=CARTESIAN_POINT('Origin',(0.,0.,0.));
#13580=CARTESIAN_POINT('',(-0.1461301977291,-5.61458017395017E-5,0.766065504584291));
#13581=CARTESIAN_POINT('',(-0.14612241379348,-4.54149644099216E-5,0.758934495415711));
#13582=CARTESIAN_POINT('',(-0.14635,-1.79227059055215E-17,0.));
#13583=CARTESIAN_POINT('Ctrl Pts',(-0.1461301977291,-5.61458017395017E-5,
0.766065504584291));
#13584=CARTESIAN_POINT('Ctrl Pts',(-0.14603380141711,0.0278870014676159,
0.764551403227483));
#13585=CARTESIAN_POINT('Ctrl Pts',(-0.138327245009168,0.0558793842949389,
0.763037301870675));
#13586=CARTESIAN_POINT('Ctrl Pts',(-0.123350675409043,0.079203679241543,
0.761523200513867));
#13587=CARTESIAN_POINT('Ctrl Pts',(-0.0971747899961838,0.119969628197767,
0.758876870634766));
#13588=CARTESIAN_POINT('Ctrl Pts',(-0.048790709571801,0.146475657227381,
0.756230540755664));
#13589=CARTESIAN_POINT('Ctrl Pts',(-0.000344588961360588,0.146589539830481,
0.753584210876561));
#13590=CARTESIAN_POINT('Ctrl Pts',(0.0481015316490792,0.14670342243358,
0.750937880997459));
#13591=CARTESIAN_POINT('Ctrl Pts',(0.0966096924455767,0.120425158610167,
0.748291551118357));
#13592=CARTESIAN_POINT('Ctrl Pts',(0.122976945064223,0.0797827231418903,
0.745645221239255));
#13593=CARTESIAN_POINT('Ctrl Pts',(0.149344197682869,0.0391402876736125,
0.742998891360154));
#13594=CARTESIAN_POINT('Ctrl Pts',(0.153570542123663,-0.01586631943953,
0.740352561481052));
#13595=CARTESIAN_POINT('Ctrl Pts',(0.133721514043982,-0.0600597087159893,
0.73770623160195));
#13596=CARTESIAN_POINT('Ctrl Pts',(0.113872485964301,-0.104253097992448,
0.735059901722848));
#13597=CARTESIAN_POINT('Ctrl Pts',(0.0699480853641458,-0.137633269432224,
0.732413571843746));
#13598=CARTESIAN_POINT('Ctrl Pts',(0.0220532014503509,-0.144921593405036,
0.729767241964644));
#13599=CARTESIAN_POINT('Ctrl Pts',(-0.0258416824634434,-0.152209917377848,
0.727120912085542));
#13600=CARTESIAN_POINT('Ctrl Pts',(-0.0777070496908773,-0.133406393883698,
0.724474582206441));
#13601=CARTESIAN_POINT('Ctrl Pts',(-0.109803305666473,-0.0971176914572187,
0.721828252327339));
#13602=CARTESIAN_POINT('Ctrl Pts',(-0.133101311474982,-0.0707764758164216,
0.71990733641299));
#13603=CARTESIAN_POINT('Ctrl Pts',(-0.14598295937539,-0.0352223077304616,
0.71798642049864));
#13604=CARTESIAN_POINT('Ctrl Pts',(-0.146290249280603,0.000131112932912382,
0.716065504584291));
#13605=CARTESIAN_POINT('Ctrl Pts',(-0.146307221518699,0.000133045872591754,
0.708934495415711));
#13606=CARTESIAN_POINT('Ctrl Pts',(-0.145987367488279,-0.0358102803178394,
0.710888040627207));
#13607=CARTESIAN_POINT('Ctrl Pts',(-0.132622002370819,-0.0719663061161047,
0.712841585838703));
#13608=CARTESIAN_POINT('Ctrl Pts',(-0.1086007072861,-0.0984612847532928,
0.7147951310502));
#13609=CARTESIAN_POINT('Ctrl Pts',(-0.0760477256663158,-0.134366532557423,
0.71744252042446));
#13610=CARTESIAN_POINT('Ctrl Pts',(-0.0239252288417074,-0.152529358077047,
0.720089909798719));
#13611=CARTESIAN_POINT('Ctrl Pts',(0.0238920022682765,-0.144630254255197,
0.722737299172979));
#13612=CARTESIAN_POINT('Ctrl Pts',(0.071709233378259,-0.136731150433346,
0.725384688547239));
#13613=CARTESIAN_POINT('Ctrl Pts',(0.115221198773618,-0.102770117270024,
0.7280320779215));
#13614=CARTESIAN_POINT('Ctrl Pts',(0.134497183226257,-0.058303052428779,
0.730679467295759));
#13615=CARTESIAN_POINT('Ctrl Pts',(0.153773167678896,-0.0138359875875333,
0.733326856670019));
#13616=CARTESIAN_POINT('Ctrl Pts',(0.148813171188813,0.0411371089316358,
0.735974246044279));
#13617=CARTESIAN_POINT('Ctrl Pts',(0.121889126928366,0.0814357351225549,
0.738621635418539));
#13618=CARTESIAN_POINT('Ctrl Pts',(0.0949650826679194,0.121734361313473,
0.741269024792799));
#13619=CARTESIAN_POINT('Ctrl Pts',(0.0460769906371109,0.147358517176143,
0.74391641416706));
#13620=CARTESIAN_POINT('Ctrl Pts',(-0.00238189178169058,0.146571023090686,
0.74656380354132));
#13621=CARTESIAN_POINT('Ctrl Pts',(-0.0508407742004934,0.14578352900523,
0.74921119291558));
#13622=CARTESIAN_POINT('Ctrl Pts',(-0.0988704470072894,0.118584384971644,
0.751858582289839));
#13623=CARTESIAN_POINT('Ctrl Pts',(-0.124470852918682,0.0774321960944291,
0.754505971664099));
#13624=CARTESIAN_POINT('Ctrl Pts',(-0.138745545153454,0.0544858868428234,
0.75598214624797));
#13625=CARTESIAN_POINT('Ctrl Pts',(-0.146046671909043,0.027201385339783,
0.757458320831841));
#13626=CARTESIAN_POINT('Ctrl Pts',(-0.14612241379348,-4.54149644099216E-5,
0.758934495415711));
#13627=CARTESIAN_POINT('Origin',(0.,0.,0.));
#13628=CARTESIAN_POINT('',(-0.146495788566881,-0.000101744904923998,0.816065504584291));
#13629=CARTESIAN_POINT('',(-0.146473871348434,-0.000110945968026819,0.808934495415711));
#13630=CARTESIAN_POINT('',(-0.14635,-1.79227059055215E-17,0.));
#13631=CARTESIAN_POINT('Ctrl Pts',(-0.146495788566881,-0.000101744904923998,
0.816065504584291));
#13632=CARTESIAN_POINT('Ctrl Pts',(-0.14616118452328,0.0421270051992108,
0.813762715835428));
#13633=CARTESIAN_POINT('Ctrl Pts',(-0.126905337350145,0.0846218946815527,
0.811459927086565));
#13634=CARTESIAN_POINT('Ctrl Pts',(-0.0947343415465314,0.111866064832055,
0.809157138337701));
#13635=CARTESIAN_POINT('Ctrl Pts',(-0.0577639214515077,0.143174651664521,
0.806510808458599));
#13636=CARTESIAN_POINT('Ctrl Pts',(-0.00373742343573488,0.154342745753647,
0.803864478579497));
#13637=CARTESIAN_POINT('Ctrl Pts',(0.0426163743729279,0.140258534729872,
0.801218148700395));
#13638=CARTESIAN_POINT('Ctrl Pts',(0.0889701721815907,0.126174323706097,
0.798571818821294));
#13639=CARTESIAN_POINT('Ctrl Pts',(0.127651269783143,0.0868378075694234,
0.795925488942192));
#13640=CARTESIAN_POINT('Ctrl Pts',(0.140954720244851,0.040253928627653,
0.79327915906309));
#13641=CARTESIAN_POINT('Ctrl Pts',(0.154258170706558,-0.00632995031411615,
0.790632829183988));
#13642=CARTESIAN_POINT('Ctrl Pts',(0.14218397402842,-0.060161192060982,
0.787986499304886));
#13643=CARTESIAN_POINT('Ctrl Pts',(0.110258679990485,-0.0966003903512828,
0.785340169425784));
#13644=CARTESIAN_POINT('Ctrl Pts',(0.0783333859525485,-0.133039588641585,
0.782693839546682));
#13645=CARTESIAN_POINT('Ctrl Pts',(0.0265569945548152,-0.152086743475322,
0.780047509667581));
#13646=CARTESIAN_POINT('Ctrl Pts',(-0.021371625274328,-0.14502367242074,
0.777401179788479));
#13647=CARTESIAN_POINT('Ctrl Pts',(-0.0693002451034712,-0.137960601366157,
0.774754849909377));
#13648=CARTESIAN_POINT('Ctrl Pts',(-0.113381093364023,-0.104787304423254,
0.772108520030274));
#13649=CARTESIAN_POINT('Ctrl Pts',(-0.133437672293631,-0.0606877215103841,
0.769462190151172));
#13650=CARTESIAN_POINT('Ctrl Pts',(-0.1420188514214,-0.0418197768941368,
0.768329961628878));
#13651=CARTESIAN_POINT('Ctrl Pts',(-0.146202281842484,-0.0209517273285418,
0.767197733106584));
#13652=CARTESIAN_POINT('Ctrl Pts',(-0.1461301977291,-5.61458017395017E-5,
0.766065504584291));
#13653=CARTESIAN_POINT('Ctrl Pts',(-0.14612241379348,-4.54149644099216E-5,
0.758934495415711));
#13654=CARTESIAN_POINT('Ctrl Pts',(-0.146182508321779,-0.0216633562673834,
0.760105710206101));
#13655=CARTESIAN_POINT('Ctrl Pts',(-0.141694203021096,-0.0432575645610501,
0.76127692499649));
#13656=CARTESIAN_POINT('Ctrl Pts',(-0.132531725405586,-0.0626424774360703,
0.76244813978688));
#13657=CARTESIAN_POINT('Ctrl Pts',(-0.111821052965107,-0.106459728368519,
0.76509552916114));
#13658=CARTESIAN_POINT('Ctrl Pts',(-0.067228569068158,-0.138988996512573,
0.767742918535399));
#13659=CARTESIAN_POINT('Ctrl Pts',(-0.0191799219195066,-0.145330206128911,
0.770390307909659));
#13660=CARTESIAN_POINT('Ctrl Pts',(0.0288687252291434,-0.151671415745249,
0.773037697283919));
#13661=CARTESIAN_POINT('Ctrl Pts',(0.080373535629496,-0.131824566833873,
0.77568508665818));
#13662=CARTESIAN_POINT('Ctrl Pts',(0.111742660473083,-0.0948805356683208,
0.77833247603244));
#13663=CARTESIAN_POINT('Ctrl Pts',(0.14311178531667,-0.0579365045027684,
0.7809798654067));
#13664=CARTESIAN_POINT('Ctrl Pts',(0.154345224603492,-0.00389529108304171,
0.783627254780959));
#13665=CARTESIAN_POINT('Ctrl Pts',(0.140297486112651,0.0424894529122293,
0.786274644155219));
#13666=CARTESIAN_POINT('Ctrl Pts',(0.126249747621811,0.0888741969075009,
0.788922033529479));
#13667=CARTESIAN_POINT('Ctrl Pts',(0.0869208313533056,0.127602471478316,
0.79156942290374));
#13668=CARTESIAN_POINT('Ctrl Pts',(0.0403254011646538,0.140934737517831,
0.794216812278));
#13669=CARTESIAN_POINT('Ctrl Pts',(-0.00627002902399674,0.154267003557346,
0.79686420165226));
#13670=CARTESIAN_POINT('Ctrl Pts',(-0.0601319731327944,0.142203261065564,
0.799511591026519));
#13671=CARTESIAN_POINT('Ctrl Pts',(-0.0965888940360299,0.110269323781398,
0.802158980400779));
#13672=CARTESIAN_POINT('Ctrl Pts',(-0.127690529151203,0.0830262752573849,
0.804417485405756));
#13673=CARTESIAN_POINT('Ctrl Pts',(-0.146124951115714,0.0413218847513699,
0.806675990410734));
#13674=CARTESIAN_POINT('Ctrl Pts',(-0.146473871348434,-0.000110945968026819,
0.808934495415711));
#13675=CARTESIAN_POINT('Origin',(0.,0.,0.));
#13676=CARTESIAN_POINT('',(-0.146444331750498,0.000119944961782359,0.866065504584291));
#13677=CARTESIAN_POINT('',(-0.146471560192382,0.00011177640072981,0.858934495415711));
#13678=CARTESIAN_POINT('',(-0.14635,-1.79227059055215E-17,0.));
#13679=CARTESIAN_POINT('Ctrl Pts',(-0.146444331750498,0.000119944961782359,
0.866065504584291));
#13680=CARTESIAN_POINT('Ctrl Pts',(-0.146516681599632,0.00829054204730037,
0.865620358322474));
#13681=CARTESIAN_POINT('Ctrl Pts',(-0.145891801779796,0.0164500693154795,
0.865175212060658));
#13682=CARTESIAN_POINT('Ctrl Pts',(-0.14453063157077,0.0244848619971339,
0.864730065798841));
#13683=CARTESIAN_POINT('Ctrl Pts',(-0.136438672357208,0.0722505376181754,
0.862083735919739));
#13684=CARTESIAN_POINT('Ctrl Pts',(-0.102325254887189,0.115607931012472,
0.859437406040638));
#13685=CARTESIAN_POINT('Ctrl Pts',(-0.0578046270350215,0.134711681091902,
0.856791076161536));
#13686=CARTESIAN_POINT('Ctrl Pts',(-0.0132839991828526,0.153815431171333,
0.854144746282434));
#13687=CARTESIAN_POINT('Ctrl Pts',(0.0416438390514653,0.148665537935894,
0.851498416403331));
#13688=CARTESIAN_POINT('Ctrl Pts',(0.081837551941475,0.121619188541491,
0.848852086524229));
#13689=CARTESIAN_POINT('Ctrl Pts',(0.122031264831484,0.0945728391470885,
0.846205756645128));
#13690=CARTESIAN_POINT('Ctrl Pts',(0.147490852377186,0.0456300335937214,
0.843559426766026));
#13691=CARTESIAN_POINT('Ctrl Pts',(0.146563060809277,-0.0028073360113171,
0.840913096886925));
#13692=CARTESIAN_POINT('Ctrl Pts',(0.145635269241369,-0.0512447056163556,
0.838266767007823));
#13693=CARTESIAN_POINT('Ctrl Pts',(0.118320098559852,-0.0991766392730661,
0.835620437128721));
#13694=CARTESIAN_POINT('Ctrl Pts',(0.0771201321287374,-0.124663936845065,
0.832974107249619));
#13695=CARTESIAN_POINT('Ctrl Pts',(0.035920165697623,-0.150151234417064,
0.830327777370517));
#13696=CARTESIAN_POINT('Ctrl Pts',(-0.0191645964830881,-0.153193895904352,
0.827681447491415));
#13697=CARTESIAN_POINT('Ctrl Pts',(-0.0629209921278279,-0.132399247274726,
0.825035117612313));
#13698=CARTESIAN_POINT('Ctrl Pts',(-0.106677387772568,-0.111604598645101,
0.822388787733211));
#13699=CARTESIAN_POINT('Ctrl Pts',(-0.139105416881337,-0.0669726398985626,
0.819742457854109));
#13700=CARTESIAN_POINT('Ctrl Pts',(-0.145362260348583,-0.0189321207373897,
0.817096127975007));
#13701=CARTESIAN_POINT('Ctrl Pts',(-0.146174510965348,-0.0126955988357878,
0.816752586844768));
#13702=CARTESIAN_POINT('Ctrl Pts',(-0.146545706411658,-0.00640163348415362,
0.81640904571453));
#13703=CARTESIAN_POINT('Ctrl Pts',(-0.146495788566881,-0.000101744904923998,
0.816065504584291));
#13704=CARTESIAN_POINT('Ctrl Pts',(-0.146473871348434,-0.000110945968026819,
0.808934495415711));
#13705=CARTESIAN_POINT('Ctrl Pts',(-0.146533950748007,-0.00724512552769256,
0.809323379784994));
#13706=CARTESIAN_POINT('Ctrl Pts',(-0.146057826922151,-0.0143712538186879,
0.809712264154277));
#13707=CARTESIAN_POINT('Ctrl Pts',(-0.145017839345608,-0.0214141189368497,
0.81010114852356));
#13708=CARTESIAN_POINT('Ctrl Pts',(-0.137937966054276,-0.0693594922943736,
0.81274853789782));
#13709=CARTESIAN_POINT('Ctrl Pts',(-0.104726321773939,-0.113446106932874,
0.81539592727208));
#13710=CARTESIAN_POINT('Ctrl Pts',(-0.0605955455659204,-0.133480028752914,
0.818043316646339));
#13711=CARTESIAN_POINT('Ctrl Pts',(-0.0164647693578984,-0.153513950572954,
0.820690706020599));
#13712=CARTESIAN_POINT('Ctrl Pts',(0.0385851387778066,-0.149495179574532,
0.823338095394859));
#13713=CARTESIAN_POINT('Ctrl Pts',(0.0793384931690736,-0.12326451930694,
0.825985484769119));
#13714=CARTESIAN_POINT('Ctrl Pts',(0.120091847560339,-0.0970338590393495,
0.828632874143379));
#13715=CARTESIAN_POINT('Ctrl Pts',(0.146548648207165,-0.0485913095025905,
0.83128026351764));
#13716=CARTESIAN_POINT('Ctrl Pts',(0.146590321408106,-0.000126046730599388,
0.833927652891899));
#13717=CARTESIAN_POINT('Ctrl Pts',(0.146631994609047,0.0483392160413931,
0.836575042266159));
#13718=CARTESIAN_POINT('Ctrl Pts',(0.120258540364101,0.0968271920486179,
0.839222431640419));
#13719=CARTESIAN_POINT('Ctrl Pts',(0.0795503554414038,0.123127897600245,
0.841869821014679));
#13720=CARTESIAN_POINT('Ctrl Pts',(0.0388421705187073,0.149428603151872,
0.844517210388939));
#13721=CARTESIAN_POINT('Ctrl Pts',(-0.0162007450817403,0.153542038247903,
0.8471645997632));
#13722=CARTESIAN_POINT('Ctrl Pts',(-0.0603659086281491,0.133584038319734,
0.84981198913746));
#13723=CARTESIAN_POINT('Ctrl Pts',(-0.104531072174558,0.113626038391565,
0.85245937851172));
#13724=CARTESIAN_POINT('Ctrl Pts',(-0.137818483666928,0.0695966034391962,
0.855106767885979));
#13725=CARTESIAN_POINT('Ctrl Pts',(-0.144980798768897,0.0216634763286692,
0.857754157260239));
#13726=CARTESIAN_POINT('Ctrl Pts',(-0.146045237806912,0.0145398171508471,
0.858147603312063));
#13727=CARTESIAN_POINT('Ctrl Pts',(-0.146532654486068,0.00732993751956911,
0.858541049363887));
#13728=CARTESIAN_POINT('Ctrl Pts',(-0.146471560192382,0.00011177640072981,
0.858934495415711));
#13729=CARTESIAN_POINT('Origin',(0.,0.,0.));
#13730=CARTESIAN_POINT('',(-0.146114231148477,2.69008449349656E-5,0.916065504584291));
#13731=CARTESIAN_POINT('',(-0.146121644853617,4.41067432152685E-5,0.908934495415711));
#13732=CARTESIAN_POINT('',(-0.14635,-1.79227059055215E-17,0.));
#13733=CARTESIAN_POINT('Ctrl Pts',(-0.146114231148477,2.69008449349656E-5,
0.916065504584291));
#13734=CARTESIAN_POINT('Ctrl Pts',(-0.146151635159142,0.0228038459942234,
0.914831670930419));
#13735=CARTESIAN_POINT('Ctrl Pts',(-0.141147538069067,0.0455652341090756,
0.913597837276548));
#13736=CARTESIAN_POINT('Ctrl Pts',(-0.131015765267123,0.0657531838068269,
0.912364003622676));
#13737=CARTESIAN_POINT('Ctrl Pts',(-0.109285110563454,0.109052354902802,
0.909717673743574));
#13738=CARTESIAN_POINT('Ctrl Pts',(-0.0639662294071284,0.140513248471977,
0.907071343864472));
#13739=CARTESIAN_POINT('Ctrl Pts',(-0.015802286694576,0.145735718560985,
0.90442501398537));
#13740=CARTESIAN_POINT('Ctrl Pts',(0.0323616560179757,0.150958188649994,
0.901778684106268));
#13741=CARTESIAN_POINT('Ctrl Pts',(0.0833706602867547,0.129942235258839,
0.899132354227166));
#13742=CARTESIAN_POINT('Ctrl Pts',(0.113877102345416,0.0923071908936453,
0.896486024348064));
#13743=CARTESIAN_POINT('Ctrl Pts',(0.144383544404078,0.0546721465284523,
0.893839694468962));
#13744=CARTESIAN_POINT('Ctrl Pts',(0.15438742425262,0.000418011189221586,
0.891193364589861));
#13745=CARTESIAN_POINT('Ctrl Pts',(0.139309808695705,-0.0456222438118789,
0.888547034710759));
#13746=CARTESIAN_POINT('Ctrl Pts',(0.124232193138789,-0.0916624988129813,
0.885900704831657));
#13747=CARTESIAN_POINT('Ctrl Pts',(0.0840730821764119,-0.129488873475953,
0.883254374952555));
#13748=CARTESIAN_POINT('Ctrl Pts',(0.0372139327097935,-0.141787641004198,
0.880608045073453));
#13749=CARTESIAN_POINT('Ctrl Pts',(-0.00964521675682358,-0.154086408532443,
0.877961715194351));
#13750=CARTESIAN_POINT('Ctrl Pts',(-0.0632044047276821,-0.140857568925962,
0.875315385315249));
#13751=CARTESIAN_POINT('Ctrl Pts',(-0.0989487482345592,-0.108156170198829,
0.872669055436147));
#13752=CARTESIAN_POINT('Ctrl Pts',(-0.128680439645858,-0.0809555616469925,
0.870467871818862));
#13753=CARTESIAN_POINT('Ctrl Pts',(-0.146086572253705,-0.0402824710322022,
0.868266688201576));
#13754=CARTESIAN_POINT('Ctrl Pts',(-0.146444331750498,0.000119944961782359,
0.866065504584291));
#13755=CARTESIAN_POINT('Ctrl Pts',(-0.146471560192382,0.00011177640072981,
0.858934495415711));
#13756=CARTESIAN_POINT('Ctrl Pts',(-0.146121567926216,-0.0412390669452651,
0.861188438738147));
#13757=CARTESIAN_POINT('Ctrl Pts',(-0.127770397964496,-0.0828616943330661,
0.863442382060584));
#13758=CARTESIAN_POINT('Ctrl Pts',(-0.096778382793969,-0.110103055552942,
0.86569632538302));
#13759=CARTESIAN_POINT('Ctrl Pts',(-0.0603764330055066,-0.142099641055337,
0.86834371475728));
#13760=CARTESIAN_POINT('Ctrl Pts',(-0.00653531471701479,-0.154255992791443,
0.870991104131539));
#13761=CARTESIAN_POINT('Ctrl Pts',(0.040082974241256,-0.14100387723139,
0.873638493505799));
#13762=CARTESIAN_POINT('Ctrl Pts',(0.0867012631995282,-0.127751761671338,
0.876285882880059));
#13763=CARTESIAN_POINT('Ctrl Pts',(0.12609672282758,-0.0890911788151255,
0.878933272254319));
#13764=CARTESIAN_POINT('Ctrl Pts',(0.140224208991091,-0.042730661487191,
0.88158066162858));
#13765=CARTESIAN_POINT('Ctrl Pts',(0.154351695154603,0.00362985584074295,
0.88422805100284));
#13766=CARTESIAN_POINT('Ctrl Pts',(0.143211207853577,0.057690307640398,
0.886875440377099));
#13767=CARTESIAN_POINT('Ctrl Pts',(0.111905662524754,0.09468823006692,0.889522829751359));
#13768=CARTESIAN_POINT('Ctrl Pts',(0.0806001171959318,0.131686152493442,
0.892170219125619));
#13769=CARTESIAN_POINT('Ctrl Pts',(0.0291295138393125,0.15162154554683,
0.894817608499879));
#13770=CARTESIAN_POINT('Ctrl Pts',(-0.0189299673197759,0.145362975188259,
0.897464997874139));
#13771=CARTESIAN_POINT('Ctrl Pts',(-0.0669894484788628,0.139104404829688,
0.9001123872484));
#13772=CARTESIAN_POINT('Ctrl Pts',(-0.11163780744042,0.10665187105916,0.902759776622659));
#13773=CARTESIAN_POINT('Ctrl Pts',(-0.132423802349956,0.0628703013313112,
0.905407165996919));
#13774=CARTESIAN_POINT('Ctrl Pts',(-0.141655418982822,0.043425734493323,
0.90658294246985));
#13775=CARTESIAN_POINT('Ctrl Pts',(-0.146180218154578,0.0217465313827003,
0.907758718942781));
#13776=CARTESIAN_POINT('Ctrl Pts',(-0.146121644853617,4.41067432152685E-5,
0.908934495415711));
#13777=CARTESIAN_POINT('Origin',(0.,0.,0.));
#13778=CARTESIAN_POINT('',(-0.146345621585321,-0.000133809880645736,0.966065504584291));
#13779=CARTESIAN_POINT('',(-0.146309694201085,-0.000133223314395004,0.958934495415711));
#13780=CARTESIAN_POINT('',(-0.14635,-1.79227059055215E-17,0.));
#13781=CARTESIAN_POINT('Ctrl Pts',(-0.146345621585321,-0.000133809880645736,
0.966065504584291));
#13782=CARTESIAN_POINT('Ctrl Pts',(-0.146004672532387,0.0370537288701324,
0.964042983538364));
#13783=CARTESIAN_POINT('Ctrl Pts',(-0.131578083002406,0.0744765756810296,
0.962020462492437));
#13784=CARTESIAN_POINT('Ctrl Pts',(-0.106003654037246,0.101251356830495,
0.959997941446511));
#13785=CARTESIAN_POINT('Ctrl Pts',(-0.0725412702228666,0.136284319036219,
0.957351611567409));
#13786=CARTESIAN_POINT('Ctrl Pts',(-0.0199938687303381,0.153087872523943,
0.954705281688306));
#13787=CARTESIAN_POINT('Ctrl Pts',(0.0275867780614433,0.143970766496025,
0.952058951809204));
#13788=CARTESIAN_POINT('Ctrl Pts',(0.0751674248532248,0.134853660468108,
0.949412621930102));
#13789=CARTESIAN_POINT('Ctrl Pts',(0.11778131694426,0.0998158949245492,
0.946766292051));
#13790=CARTESIAN_POINT('Ctrl Pts',(0.135923405490256,0.0548948063954655,
0.944119962171899));
#13791=CARTESIAN_POINT('Ctrl Pts',(0.154065494036253,0.0099737178663825,
0.941473632292797));
#13792=CARTESIAN_POINT('Ctrl Pts',(0.147735779037212,-0.0448306936482241,
0.938827302413695));
#13793=CARTESIAN_POINT('Ctrl Pts',(0.119831470632095,-0.0844335867733556,
0.936180972534593));
#13794=CARTESIAN_POINT('Ctrl Pts',(0.0919271622269763,-0.124036479898489,
0.933534642655491));
#13795=CARTESIAN_POINT('Ctrl Pts',(0.0424482604157787,-0.148437854634144,
0.93088831277639));
#13796=CARTESIAN_POINT('Ctrl Pts',(-0.00595796300272124,-0.146468817862788,
0.928241982897288));
#13797=CARTESIAN_POINT('Ctrl Pts',(-0.0543641864212212,-0.144499781091432,
0.925595653018186));
#13798=CARTESIAN_POINT('Ctrl Pts',(-0.101697731447024,-0.116160332813065,
0.922949323139084));
#13799=CARTESIAN_POINT('Ctrl Pts',(-0.126293289834417,-0.0744218843624929,
0.920302993259982));
#13800=CARTESIAN_POINT('Ctrl Pts',(-0.139421333187579,-0.052143709087005,
0.918890497034752));
#13801=CARTESIAN_POINT('Ctrl Pts',(-0.146071410932229,-0.0260482098028304,
0.917478000809521));
#13802=CARTESIAN_POINT('Ctrl Pts',(-0.146114231148477,2.69008449349656E-5,
0.916065504584291));
#13803=CARTESIAN_POINT('Ctrl Pts',(-0.146121644853617,4.41067432152685E-5,
0.908934495415711));
#13804=CARTESIAN_POINT('Ctrl Pts',(-0.146048333958771,-0.027118852224649,
0.910406108317041));
#13805=CARTESIAN_POINT('Ctrl Pts',(-0.138795050353101,-0.0543181883240968,
0.91187772121837));
#13806=CARTESIAN_POINT('Ctrl Pts',(-0.124603830013468,-0.0772180274565794,
0.9133493341197));
#13807=CARTESIAN_POINT('Ctrl Pts',(-0.0990742319099257,-0.118414180831446,
0.91599672349396));
#13808=CARTESIAN_POINT('Ctrl Pts',(-0.0510914048453256,-0.145695881896007,
0.91864411286822));
#13809=CARTESIAN_POINT('Ctrl Pts',(-0.00263394834681351,-0.146566710184873,
0.92129150224248));
#13810=CARTESIAN_POINT('Ctrl Pts',(0.0458235081516972,-0.147437538473739,
0.92393889161674));
#13811=CARTESIAN_POINT('Ctrl Pts',(0.0947555940841207,-0.121897493986912,
0.926586280990999));
#13812=CARTESIAN_POINT('Ctrl Pts',(0.121748900601314,-0.0816452290135895,
0.929233670365259));
#13813=CARTESIAN_POINT('Ctrl Pts',(0.148742207118509,-0.0413929640402651,
0.931881059739519));
#13814=CARTESIAN_POINT('Ctrl Pts',(0.153796734220472,0.0135715214195569,
0.93452844911378));
#13815=CARTESIAN_POINT('Ctrl Pts',(0.134597248858856,0.0580716696672091,
0.93717583848804));
#13816=CARTESIAN_POINT('Ctrl Pts',(0.115397763497239,0.102571817914861,
0.9398232278623));
#13817=CARTESIAN_POINT('Ctrl Pts',(0.0719442656720451,0.136607628950342,
0.942470617236559));
#13818=CARTESIAN_POINT('Ctrl Pts',(0.0241406894609324,0.144588953003544,
0.945118006610819));
#13819=CARTESIAN_POINT('Ctrl Pts',(-0.023662886750181,0.152570277056746,
0.947765395985079));
#13820=CARTESIAN_POINT('Ctrl Pts',(-0.0758165413472122,0.134497114127667,
0.950412785359339));
#13821=CARTESIAN_POINT('Ctrl Pts',(-0.108431221550465,0.0986479012011113,
0.953060174733599));
#13822=CARTESIAN_POINT('Ctrl Pts',(-0.132554242808212,0.0721325001574252,
0.955018281627637));
#13823=CARTESIAN_POINT('Ctrl Pts',(-0.145988218858404,0.0358924841874147,
0.956976388521674));
#13824=CARTESIAN_POINT('Ctrl Pts',(-0.146309694201085,-0.000133223314395004,
0.958934495415711));
#13825=CARTESIAN_POINT('Origin',(0.,0.,0.));
#13826=CARTESIAN_POINT('',(-0.146565171121453,5.44893591410845E-5,1.01606550458429));
#13827=CARTESIAN_POINT('',(-0.146582076026177,3.15354312248815E-5,1.00893449541571));
#13828=CARTESIAN_POINT('',(-0.14635,-1.79227059055215E-17,0.));
#13829=CARTESIAN_POINT('Ctrl Pts',(-0.146565171121453,5.44893591410845E-5,
1.01606550458429));
#13830=CARTESIAN_POINT('Ctrl Pts',(-0.146579596851449,0.00307427920823236,
1.01590062602541));
#13831=CARTESIAN_POINT('Ctrl Pts',(-0.146494352296349,0.00609323927190738,
1.01573574746653));
#13832=CARTESIAN_POINT('Ctrl Pts',(-0.146306854564556,0.00910583530985269,
1.01557086890765));
#13833=CARTESIAN_POINT('Ctrl Pts',(-0.143297482980539,0.0574585317612167,
1.01292453902855));
#13834=CARTESIAN_POINT('Ctrl Pts',(-0.11394685994478,0.104171803331984,
1.01027820914945));
#13835=CARTESIAN_POINT('Ctrl Pts',(-0.0716892273871119,0.127864250695428,
1.00763187927034));
#13836=CARTESIAN_POINT('Ctrl Pts',(-0.0294315948294418,0.151556698058874,
1.00498554939124));
#13837=CARTESIAN_POINT('Ctrl Pts',(0.0257330472501378,0.152228321214993,
1.00233921951214));
#13838=CARTESIAN_POINT('Ctrl Pts',(0.0685549742796134,0.129571707678744,
0.999692889633039));
#13839=CARTESIAN_POINT('Ctrl Pts',(0.111376901309088,0.106915094142495,
0.997046559753937));
#13840=CARTESIAN_POINT('Ctrl Pts',(0.141856113288459,0.0609302439138786,
0.994400229874835));
#13841=CARTESIAN_POINT('Ctrl Pts',(0.146041795372579,0.0126651464112397,
0.991753899995733));
#13842=CARTESIAN_POINT('Ctrl Pts',(0.150227477456699,-0.0355999510913994,
0.989107570116631));
#13843=CARTESIAN_POINT('Ctrl Pts',(0.128119629645567,-0.0861452958680607,
0.986461240237529));
#13844=CARTESIAN_POINT('Ctrl Pts',(0.0898373616998479,-0.115835488396583,
0.983814910358427));
#13845=CARTESIAN_POINT('Ctrl Pts',(0.051555093754129,-0.145525680925106,
0.981168580479325));
#13846=CARTESIAN_POINT('Ctrl Pts',(-0.00290159432617693,-0.154360721205491,
0.978522250600224));
#13847=CARTESIAN_POINT('Ctrl Pts',(-0.0486070196525971,-0.138296672301818,
0.975875920721122));
#13848=CARTESIAN_POINT('Ctrl Pts',(-0.0943124449790173,-0.122232623398145,
0.97322959084202));
#13849=CARTESIAN_POINT('Ctrl Pts',(-0.131266607551552,-0.081269485310415,
0.970583260962917));
#13850=CARTESIAN_POINT('Ctrl Pts',(-0.142555005769704,-0.0341567308046872,
0.967936931083816));
#13851=CARTESIAN_POINT('Ctrl Pts',(-0.145215975052668,-0.0230510282813687,
0.967313122250641));
#13852=CARTESIAN_POINT('Ctrl Pts',(-0.146450780951306,-0.0116036114945705,
0.966689313417466));
#13853=CARTESIAN_POINT('Ctrl Pts',(-0.146345621585321,-0.000133809880645736,
0.966065504584291));
#13854=CARTESIAN_POINT('Ctrl Pts',(-0.146309694201085,-0.000133223314395004,
0.958934495415711));
#13855=CARTESIAN_POINT('Ctrl Pts',(-0.146422858258782,-0.0128148032088542,
0.959623777895933));
#13856=CARTESIAN_POINT('Ctrl Pts',(-0.14491119500038,-0.0254698272036438,
0.960313060376156));
#13857=CARTESIAN_POINT('Ctrl Pts',(-0.141668994059001,-0.037664762585484,
0.961002342856379));
#13858=CARTESIAN_POINT('Ctrl Pts',(-0.129216380554811,-0.0845029505214961,
0.963649732230639));
#13859=CARTESIAN_POINT('Ctrl Pts',(-0.0912354477369537,-0.12455406346949,
0.966297121604899));
#13860=CARTESIAN_POINT('Ctrl Pts',(-0.0451234138007503,-0.1394726343957,
0.968944510979159));
#13861=CARTESIAN_POINT('Ctrl Pts',(0.00098862013545236,-0.154391205321909,
0.97159190035342));
#13862=CARTESIAN_POINT('Ctrl Pts',(0.055231755190001,-0.144177234226336,
0.974239289727679));
#13863=CARTESIAN_POINT('Ctrl Pts',(0.0927598492034174,-0.113509244531313,
0.976886679101939));
#13864=CARTESIAN_POINT('Ctrl Pts',(0.130287943216833,-0.0828412548362905,
0.979534068476199));
#13865=CARTESIAN_POINT('Ctrl Pts',(0.151100996189117,-0.0317192465418168,
0.982181457850459));
#13866=CARTESIAN_POINT('Ctrl Pts',(0.145665560755875,0.0164402745715088,
0.984828847224719));
#13867=CARTESIAN_POINT('Ctrl Pts',(0.140230125322634,0.0645997956848379,
0.987476236598979));
#13868=CARTESIAN_POINT('Ctrl Pts',(0.108546201483865,0.109796829617019,
0.990123625973239));
#13869=CARTESIAN_POINT('Ctrl Pts',(0.0651266538643092,0.131328813193254,
0.992771015347499));
#13870=CARTESIAN_POINT('Ctrl Pts',(0.0217071062447581,0.152860796769488,
0.995418404721759));
#13871=CARTESIAN_POINT('Ctrl Pts',(-0.0334480651555777,0.15072772998978,
0.998065794096019));
#13872=CARTESIAN_POINT('Ctrl Pts',(-0.0750749586823209,0.125906667008376,
1.00071318347028));
#13873=CARTESIAN_POINT('Ctrl Pts',(-0.116701852209067,0.101085604026969,
1.00336057284454));
#13874=CARTESIAN_POINT('Ctrl Pts',(-0.144800467862219,0.053576544843864,
1.0060079622188));
#13875=CARTESIAN_POINT('Ctrl Pts',(-0.146500196332402,0.00514107896046776,
1.00865535159306));
#13876=CARTESIAN_POINT('Ctrl Pts',(-0.146559936783033,0.00343871495990628,
1.00874839953394));
#13877=CARTESIAN_POINT('Ctrl Pts',(-0.146587066279139,0.00173520655478852,
1.00884144747483));
#13878=CARTESIAN_POINT('Ctrl Pts',(-0.146582076026177,3.15354312248815E-5,
1.00893449541571));
#13879=CARTESIAN_POINT('Origin',(0.,0.,0.));
#13880=CARTESIAN_POINT('',(-0.146184049129756,9.96948043307314E-5,1.06606550458429));
#13881=CARTESIAN_POINT('',(-0.146216477546812,0.000114345603752017,1.05893449541571));
#13882=CARTESIAN_POINT('',(-0.14635,-1.79227059055215E-17,0.));
#13883=CARTESIAN_POINT('Ctrl Pts',(-0.146184049129756,9.96948043307314E-5,
1.06606550458429));
#13884=CARTESIAN_POINT('Ctrl Pts',(-0.146294264763128,0.0176817746259609,
1.06511193863336));
#13885=CARTESIAN_POINT('Ctrl Pts',(-0.143360807533043,0.0352283113603788,
1.06415837268242));
#13886=CARTESIAN_POINT('Ctrl Pts',(-0.13721959397524,0.0515693218739058,
1.06320480673148));
#13887=CARTESIAN_POINT('Ctrl Pts',(-0.120176538991979,0.0969187854681546,
1.06055847685238));
#13888=CARTESIAN_POINT('Ctrl Pts',(-0.0784283132238915,0.132983650068601,
1.05791214697328));
#13889=CARTESIAN_POINT('Ctrl Pts',(-0.0310837364199337,0.143256459747686,
1.05526581709418));
#13890=CARTESIAN_POINT('Ctrl Pts',(0.0162608403840241,0.153529269426771,
1.05261948721508));
#13891=CARTESIAN_POINT('Ctrl Pts',(0.0692017682238519,0.138010024184496,
1.04997315733597));
#13892=CARTESIAN_POINT('Ctrl Pts',(0.103507151520239,0.103802126728842,
1.04732682745687));
#13893=CARTESIAN_POINT('Ctrl Pts',(0.137812534816628,0.0695942292731864,
1.04468049757777));
#13894=CARTESIAN_POINT('Ctrl Pts',(0.153482373569574,0.01669767960415,1.04203416769867));
#13895=CARTESIAN_POINT('Ctrl Pts',(0.143344336052008,-0.0306759392859165,
1.03938783781957));
#13896=CARTESIAN_POINT('Ctrl Pts',(0.133206298534443,-0.0780495581759789,
1.03674150794047));
#13897=CARTESIAN_POINT('Ctrl Pts',(0.0972603847463712,-0.119900246287072,
1.03409517806136));
#13898=CARTESIAN_POINT('Ctrl Pts',(0.0519596049571008,-0.137072285243832,
1.03144884818226));
#13899=CARTESIAN_POINT('Ctrl Pts',(0.00665882516783032,-0.154244324200591,
1.02880251830316));
#13900=CARTESIAN_POINT('Ctrl Pts',(-0.0479968206226384,-0.146737714003016,
1.02615618842406));
#13901=CARTESIAN_POINT('Ctrl Pts',(-0.0869905834517384,-0.11798834823825,
1.02350985854496));
#13902=CARTESIAN_POINT('Ctrl Pts',(-0.123554854979944,-0.0910302005802824,
1.02102840722473));
#13903=CARTESIAN_POINT('Ctrl Pts',(-0.146348061346918,-0.0453938791777224,
1.01854695590451));
#13904=CARTESIAN_POINT('Ctrl Pts',(-0.146565171121453,5.44893591410845E-5,
1.01606550458429));
#13905=CARTESIAN_POINT('Ctrl Pts',(-0.146582076026177,3.15354312248815E-5,
1.00893449541571));
#13906=CARTESIAN_POINT('Ctrl Pts',(-0.146445084172466,-0.0467374494427972,
1.01148883684909));
#13907=CARTESIAN_POINT('Ctrl Pts',(-0.122102455869861,-0.0936290599181376,
1.01404317828246));
#13908=CARTESIAN_POINT('Ctrl Pts',(-0.0837162036049941,-0.120334265578335,
1.01659751971584));
#13909=CARTESIAN_POINT('Ctrl Pts',(-0.0439316411201867,-0.14801227165006,
1.0192449090901));
#13910=CARTESIAN_POINT('Ctrl Pts',(0.0109383251366414,-0.154006411209824,
1.02189229846436));
#13911=CARTESIAN_POINT('Ctrl Pts',(0.0557604321169594,-0.135571060438576,
1.02453968783862));
#13912=CARTESIAN_POINT('Ctrl Pts',(0.100582539097277,-0.11713570966733,
1.02718707721288));
#13913=CARTESIAN_POINT('Ctrl Pts',(0.135356786801084,-0.0742708685650716,
1.02983446658714));
#13914=CARTESIAN_POINT('Ctrl Pts',(0.144154783532934,-0.0266108361928598,
1.0324818559614));
#13915=CARTESIAN_POINT('Ctrl Pts',(0.152952780264784,0.0210491961793507,
1.03512924533566));
#13916=CARTESIAN_POINT('Ctrl Pts',(0.135774526024679,0.0735044198215165,
1.03777663470992));
#13917=CARTESIAN_POINT('Ctrl Pts',(0.100488543649143,0.106727647840587,
1.04042402408418));
#13918=CARTESIAN_POINT('Ctrl Pts',(0.0652025612736062,0.139950875859659,
1.04307141345844));
#13919=CARTESIAN_POINT('Ctrl Pts',(0.0118088507626404,0.153942108255635,
1.0457188028327));
#13920=CARTESIAN_POINT('Ctrl Pts',(-0.0352355257975899,0.142292641904202,
1.04836619220696));
#13921=CARTESIAN_POINT('Ctrl Pts',(-0.0822799023578202,0.130643175552769,
1.05101358158122));
#13922=CARTESIAN_POINT('Ctrl Pts',(-0.122974944967313,0.0933530104539243,
1.05366097095548));
#13923=CARTESIAN_POINT('Ctrl Pts',(-0.138680233730631,0.0475029577050484,
1.05630836032974));
#13924=CARTESIAN_POINT('Ctrl Pts',(-0.143873300563147,0.0323423075707214,
1.05718373869173));
#13925=CARTESIAN_POINT('Ctrl Pts',(-0.146334133026589,0.0162457690968458,
1.05805911705372));
#13926=CARTESIAN_POINT('Ctrl Pts',(-0.146216477546812,0.000114345603752017,
1.05893449541571));
#13927=CARTESIAN_POINT('Origin',(0.,0.,0.));
#13928=CARTESIAN_POINT('',(-0.146204073634541,-0.000109175101205505,1.11606550458429));
#13929=CARTESIAN_POINT('',(-0.146170555016798,-9.22629125885076E-5,1.10893449541571));
#13930=CARTESIAN_POINT('',(-0.14635,-1.79227059055215E-17,0.));
#13931=CARTESIAN_POINT('Ctrl Pts',(-0.146204073634541,-0.000109175101205505,
1.11606550458429));
#13932=CARTESIAN_POINT('Ctrl Pts',(-0.145981599624502,0.032003853555373,
1.1143232512413));
#13933=CARTESIAN_POINT('Ctrl Pts',(-0.135565881201595,0.0642480963468658,
1.11258099789831));
#13934=CARTESIAN_POINT('Ctrl Pts',(-0.11609067353381,0.0895073597405865,
1.11083874455532));
#13935=CARTESIAN_POINT('Ctrl Pts',(-0.0865095427755784,0.127873963375947,
1.10819241467622));
#13936=CARTESIAN_POINT('Ctrl Pts',(-0.0360273159486943,0.150125560802435,
1.10554608479712));
#13937=CARTESIAN_POINT('Ctrl Pts',(0.0122494975033169,0.14607724579886,
1.10289975491801));
#13938=CARTESIAN_POINT('Ctrl Pts',(0.0605263109553308,0.142028930795284,
1.10025342503891));
#13939=CARTESIAN_POINT('Ctrl Pts',(0.10659771103247,0.111680703361642,1.09760709515981));
#13940=CARTESIAN_POINT('Ctrl Pts',(0.129376093089052,0.0689234246557527,
1.09496076528071));
#13941=CARTESIAN_POINT('Ctrl Pts',(0.152154475145634,0.0261661459498645,
1.09231443540161));
#13942=CARTESIAN_POINT('Ctrl Pts',(0.151639839181659,-0.0290001840282729,
1.0896681055225));
#13943=CARTESIAN_POINT('Ctrl Pts',(0.128067742174483,-0.0713250681289163,
1.0870217756434));
#13944=CARTESIAN_POINT('Ctrl Pts',(0.104495645167307,-0.11364995222956,
1.0843754457643));
#13945=CARTESIAN_POINT('Ctrl Pts',(0.0578660871169326,-0.143133390452712,
1.0817291158852));
#13946=CARTESIAN_POINT('Ctrl Pts',(0.00952215035475689,-0.146280349267719,
1.0790827860061));
#13947=CARTESIAN_POINT('Ctrl Pts',(-0.0388217864074202,-0.149427308082725,
1.07643645612699));
#13948=CARTESIAN_POINT('Ctrl Pts',(-0.0888801018813974,-0.126237787489585,
1.07379012624789));
#13949=CARTESIAN_POINT('Ctrl Pts',(-0.117740317519168,-0.0873259958989869,
1.07114379636879));
#13950=CARTESIAN_POINT('Ctrl Pts',(-0.136201180005177,-0.0624354946409797,
1.06945103244062));
#13951=CARTESIAN_POINT('Ctrl Pts',(-0.145988395071105,-0.0311118962502767,
1.06775826851246));
#13952=CARTESIAN_POINT('Ctrl Pts',(-0.146184049129756,9.96948043307314E-5,
1.06606550458429));
#13953=CARTESIAN_POINT('Ctrl Pts',(-0.146216477546812,0.000114345603752017,
1.05893449541571));
#13954=CARTESIAN_POINT('Ctrl Pts',(-0.145978309898544,-0.0325401742182177,
1.06070650642798));
#13955=CARTESIAN_POINT('Ctrl Pts',(-0.135174246449945,-0.06533764273189,
1.06247851744025));
#13956=CARTESIAN_POINT('Ctrl Pts',(-0.115079600404687,-0.0908043159161929,
1.06425052845252));
#13957=CARTESIAN_POINT('Ctrl Pts',(-0.0850581433982766,-0.128851596389654,
1.06689791782678));
#13958=CARTESIAN_POINT('Ctrl Pts',(-0.0342996944683099,-0.150536216937668,
1.06954530720104));
#13959=CARTESIAN_POINT('Ctrl Pts',(0.0139457694684962,-0.145925507476389,
1.0721926965753));
#13960=CARTESIAN_POINT('Ctrl Pts',(0.0621912334052997,-0.14131479801511,
1.07484008594956));
#13961=CARTESIAN_POINT('Ctrl Pts',(0.107923712348941,-0.110408758544542,
1.07748747532382));
#13962=CARTESIAN_POINT('Ctrl Pts',(0.1301953818052,-0.0673639426912374,
1.08013486469808));
#13963=CARTESIAN_POINT('Ctrl Pts',(0.15246705126146,-0.024319126837932,
1.08278225407234));
#13964=CARTESIAN_POINT('Ctrl Pts',(0.151277911230334,0.0308644653981125,
1.0854296434466));
#13965=CARTESIAN_POINT('Ctrl Pts',(0.127172648928576,0.0729099141598672,
1.08807703282086));
#13966=CARTESIAN_POINT('Ctrl Pts',(0.103067386626818,0.114955362921624,
1.09072442219512));
#13967=CARTESIAN_POINT('Ctrl Pts',(0.0560460020544268,0.143862668209093,
1.09337181156938));
#13968=CARTESIAN_POINT('Ctrl Pts',(0.00764670469074742,0.146390799320458,
1.09601920094364));
#13969=CARTESIAN_POINT('Ctrl Pts',(-0.0407525926729279,0.148918930431823,
1.0986665903179));
#13970=CARTESIAN_POINT('Ctrl Pts',(-0.0905298028278899,0.125067887367091,
1.10131397969216));
#13971=CARTESIAN_POINT('Ctrl Pts',(-0.11888440661962,0.0857626730052823,
1.10396136906642));
#13972=CARTESIAN_POINT('Ctrl Pts',(-0.136639133674055,0.0611510311732957,
1.10561907784952));
#13973=CARTESIAN_POINT('Ctrl Pts',(-0.145994366384503,0.0304800321277272,
1.10727678663261));
#13974=CARTESIAN_POINT('Ctrl Pts',(-0.146170555016798,-9.22629125885076E-5,
1.10893449541571));
#13975=CARTESIAN_POINT('Origin',(0.,0.,0.));
#13976=CARTESIAN_POINT('',(-0.146577386142569,-3.88073511912723E-5,1.16606550458429));
#13977=CARTESIAN_POINT('',(-0.146552328192774,-6.73160170860698E-5,1.15893449541571));
#13978=CARTESIAN_POINT('',(-0.14635,-1.79227059055215E-17,0.));
#13979=CARTESIAN_POINT('Ctrl Pts',(-0.146577386142569,-3.88073511912723E-5,
1.16606550458429));
#13980=CARTESIAN_POINT('Ctrl Pts',(-0.146413350709018,0.0463056768050285,
1.16353456384924));
#13981=CARTESIAN_POINT('Ctrl Pts',(-0.122574225104448,0.0927954474992645,
1.1610036231142));
#13982=CARTESIAN_POINT('Ctrl Pts',(-0.0847742546295189,0.119590709008994,
1.15847268237915));
#13983=CARTESIAN_POINT('Ctrl Pts',(-0.0452509303920754,0.147607604138013,
1.15582635250005));
#13984=CARTESIAN_POINT('Ctrl Pts',(0.00953524646069181,0.154093252855687,
1.15318002262095));
#13985=CARTESIAN_POINT('Ctrl Pts',(0.0545077808453859,0.136079071706768,
1.15053369274185));
#13986=CARTESIAN_POINT('Ctrl Pts',(0.0994803152300801,0.118064890557849,
1.14788736286275));
#13987=CARTESIAN_POINT('Ctrl Pts',(0.134639207146701,0.0755508795423365,
1.14524103298364));
#13988=CARTESIAN_POINT('Ctrl Pts',(0.14389167861853,0.027996370364851,1.14259470310454));
#13989=CARTESIAN_POINT('Ctrl Pts',(0.15314415009036,-0.0195581388126345,
1.13994837322544));
#13990=CARTESIAN_POINT('Ctrl Pts',(0.136490201117397,-0.0721531461520931,
1.13730204334634));
#13991=CARTESIAN_POINT('Ctrl Pts',(0.101552606157185,-0.105715089329518,
1.13465571346724));
#13992=CARTESIAN_POINT('Ctrl Pts',(0.0666150111969725,-0.139277032506943,
1.13200938358813));
#13993=CARTESIAN_POINT('Ctrl Pts',(0.0133937702495101,-0.153805911522335,
1.12936305370903));
#13994=CARTESIAN_POINT('Ctrl Pts',(-0.033750917386428,-0.142651629870951,
1.12671672382993));
#13995=CARTESIAN_POINT('Ctrl Pts',(-0.0808956050223675,-0.131497348219567,
1.12407039395083));
#13996=CARTESIAN_POINT('Ctrl Pts',(-0.121963739346782,-0.094659905901407,
1.12142406407173));
#13997=CARTESIAN_POINT('Ctrl Pts',(-0.1381577891642,-0.0490003798202082,
1.11877773419262));
#13998=CARTESIAN_POINT('Ctrl Pts',(-0.143690228857438,-0.0334015285560649,
1.11787365765651));
#13999=CARTESIAN_POINT('Ctrl Pts',(-0.146319518115206,-0.0167730178360648,
1.1169695811204));
#14000=CARTESIAN_POINT('Ctrl Pts',(-0.146204073634541,-0.000109175101205505,
1.11606550458429));
#14001=CARTESIAN_POINT('Ctrl Pts',(-0.146170555016798,-9.22629125885076E-5,
1.10893449541571));
#14002=CARTESIAN_POINT('Ctrl Pts',(-0.146275742653821,-0.0183444476975235,
1.10992417600687));
#14003=CARTESIAN_POINT('Ctrl Pts',(-0.143109248288425,-0.0365614514641733,
1.11091385659804));
#14004=CARTESIAN_POINT('Ctrl Pts',(-0.136505188007283,-0.0534328725168923,
1.1119035371892));
#14005=CARTESIAN_POINT('Ctrl Pts',(-0.118839368174718,-0.0985638180183679,
1.11455092656346));
#14006=CARTESIAN_POINT('Ctrl Pts',(-0.0765757310810901,-0.134066323362434,
1.11719831593772));
#14007=CARTESIAN_POINT('Ctrl Pts',(-0.0290731934694857,-0.143678417446031,
1.11984570531198));
#14008=CARTESIAN_POINT('Ctrl Pts',(0.01842934414212,-0.153290511529629,
1.12249309468624));
#14009=CARTESIAN_POINT('Ctrl Pts',(0.071170782271703,-0.137012194352758,
1.1251404840605));
#14010=CARTESIAN_POINT('Ctrl Pts',(0.10499283308901,-0.102299771349957,
1.12778787343476));
#14011=CARTESIAN_POINT('Ctrl Pts',(0.138814883906317,-0.0675873483471558,
1.13043526280902));
#14012=CARTESIAN_POINT('Ctrl Pts',(0.153717547411349,-0.0144408195184256,
1.13308265218328));
#14013=CARTESIAN_POINT('Ctrl Pts',(0.142874638214406,0.0327959749574983,
1.13573004155754));
#14014=CARTESIAN_POINT('Ctrl Pts',(0.132031729017462,0.0800327694334235,
1.1383774309318));
#14015=CARTESIAN_POINT('Ctrl Pts',(0.0954432471185425,0.121359829556542,
1.14102482030606));
#14016=CARTESIAN_POINT('Ctrl Pts',(0.0498685966661331,0.137847238945365,
1.14367220968032));
#14017=CARTESIAN_POINT('Ctrl Pts',(0.00429394621372511,0.154334648334189,
1.14631959905458));
#14018=CARTESIAN_POINT('Ctrl Pts',(-0.0502668727921719,0.145982406988718,
1.14896698842884));
#14019=CARTESIAN_POINT('Ctrl Pts',(-0.0888222026239048,0.116616270474356,
1.1516143778031));
#14020=CARTESIAN_POINT('Ctrl Pts',(-0.124357782404925,0.0895501633622979,
1.1540544170073));
#14021=CARTESIAN_POINT('Ctrl Pts',(-0.146296868742479,0.0446329749882746,
1.15649445621151));
#14022=CARTESIAN_POINT('Ctrl Pts',(-0.146552328192774,-6.73160170860698E-5,
1.15893449541571));
#14023=CARTESIAN_POINT('Origin',(0.,0.,0.));
#14024=CARTESIAN_POINT('',(-0.146318311025392,0.000133437649768732,1.21606550458429));
#14025=CARTESIAN_POINT('',(-0.146373054956946,0.000132657382717961,1.20893449541571));
#14026=CARTESIAN_POINT('',(-0.14635,-1.79227059055215E-17,0.));
#14027=CARTESIAN_POINT('Ctrl Pts',(-0.146318311025392,0.000133437649768732,
1.21606550458429));
#14028=CARTESIAN_POINT('Ctrl Pts',(-0.146429658069886,0.0125190846592594,
1.21539220633629));
#14029=CARTESIAN_POINT('Ctrl Pts',(-0.144988168643405,0.0248791929292086,
1.21471890808829));
#14030=CARTESIAN_POINT('Ctrl Pts',(-0.141892968227885,0.0368102906365087,
1.21404560984029));
#14031=CARTESIAN_POINT('Ctrl Pts',(-0.129727599662405,0.083704249513052,
1.21139927996119));
#14032=CARTESIAN_POINT('Ctrl Pts',(-0.0920156607298113,0.123970842060419,
1.20875295008209));
#14033=CARTESIAN_POINT('Ctrl Pts',(-0.0460184991925076,0.139179415364965,
1.20610662020299));
#14034=CARTESIAN_POINT('Ctrl Pts',(-2.13376552038805E-5,0.15438798866951,
1.20346029032389));
#14035=CARTESIAN_POINT('Ctrl Pts',(0.0542610464868107,0.144538542731236,
1.20081396044478));
#14036=CARTESIAN_POINT('Ctrl Pts',(0.091982751999895,0.114139323915075,
1.19816763056568));
#14037=CARTESIAN_POINT('Ctrl Pts',(0.129704457512977,0.0837401050989159,
1.19552130068658));
#14038=CARTESIAN_POINT('Ctrl Pts',(0.150865484397133,0.0327911134048729,
1.19287497080748));
#14039=CARTESIAN_POINT('Ctrl Pts',(0.145780097726084,-0.0153874961003253,
1.19022864092838));
#14040=CARTESIAN_POINT('Ctrl Pts',(0.140694711055036,-0.063566105605525,
1.18758231104927));
#14041=CARTESIAN_POINT('Ctrl Pts',(0.109362910828785,-0.108974332921877,
1.18493598117017));
#14042=CARTESIAN_POINT('Ctrl Pts',(0.0661257549466402,-0.130828118009858,
1.18228965129107));
#14043=CARTESIAN_POINT('Ctrl Pts',(0.0228885990644955,-0.152681903097838,
1.17964332141197));
#14044=CARTESIAN_POINT('Ctrl Pts',(-0.0322539124735426,-0.150981245957443,
1.17699699153287));
#14045=CARTESIAN_POINT('Ctrl Pts',(-0.0740621845924981,-0.126504564117865,
1.17435066165376));
#14046=CARTESIAN_POINT('Ctrl Pts',(-0.115870456711455,-0.102027882278287,
1.17170433177466));
#14047=CARTESIAN_POINT('Ctrl Pts',(-0.144344489411329,-0.0547751757395235,
1.16905800189556));
#14048=CARTESIAN_POINT('Ctrl Pts',(-0.146451269950206,-0.00637475169995868,
1.16641167201646));
#14049=CARTESIAN_POINT('Ctrl Pts',(-0.146543132875163,-0.00426432565444621,
1.1662962828724));
#14050=CARTESIAN_POINT('Ctrl Pts',(-0.146584864748453,-0.00215171749738942,
1.16618089372835));
#14051=CARTESIAN_POINT('Ctrl Pts',(-0.146577386142569,-3.88073511912723E-5,
1.16606550458429));
#14052=CARTESIAN_POINT('Ctrl Pts',(-0.146552328192774,-6.73160170860698E-5,
1.15893449541571));
#14053=CARTESIAN_POINT('Ctrl Pts',(-0.146574036680232,-0.00386586684592084,
1.15914184558577));
#14054=CARTESIAN_POINT('Ctrl Pts',(-0.1464391612665,-0.00766285139452399,
1.15934919575582));
#14055=CARTESIAN_POINT('Ctrl Pts',(-0.146142739258869,-0.0114471821958193,
1.15955654592588));
#14056=CARTESIAN_POINT('Ctrl Pts',(-0.142358105404532,-0.0597644666683822,
1.16220393530014));
#14057=CARTESIAN_POINT('Ctrl Pts',(-0.112238997038288,-0.106019003930254,
1.1648513246744));
#14058=CARTESIAN_POINT('Ctrl Pts',(-0.0695815129186611,-0.129023839960917,
1.16749871404866));
#14059=CARTESIAN_POINT('Ctrl Pts',(-0.026924028799035,-0.15202867599158,
1.17014610342292));
#14060=CARTESIAN_POINT('Ctrl Pts',(0.0282718310739737,-0.151783810791035,
1.17279349279718));
#14061=CARTESIAN_POINT('Ctrl Pts',(0.0707235276354612,-0.128401405199111,
1.17544088217144));
#14062=CARTESIAN_POINT('Ctrl Pts',(0.11317522419695,-0.105018999607187,
1.1780882715457));
#14063=CARTESIAN_POINT('Ctrl Pts',(0.142882757446916,-0.0584990536238821,
1.18073566091996));
#14064=CARTESIAN_POINT('Ctrl Pts',(0.146238551171451,-0.0101500920973681,
1.18338305029422));
#14065=CARTESIAN_POINT('Ctrl Pts',(0.149594344895986,0.0381988694291446,
1.18603043966848));
#14066=CARTESIAN_POINT('Ctrl Pts',(0.12659839909509,0.0883768464988665,
1.18867782904274));
#14067=CARTESIAN_POINT('Ctrl Pts',(0.0877840381772113,0.117399748124142,
1.191325218417));
#14068=CARTESIAN_POINT('Ctrl Pts',(0.0489696772593311,0.146422649749419,
1.19397260779126));
#14069=CARTESIAN_POINT('Ctrl Pts',(-0.00566309877553352,0.154290475930249,
1.19661999716552));
#14070=CARTESIAN_POINT('Ctrl Pts',(-0.0510896721842483,0.137399358129564,
1.19926738653978));
#14071=CARTESIAN_POINT('Ctrl Pts',(-0.0965162455929618,0.12050824032888,
1.20191477591404));
#14072=CARTESIAN_POINT('Ctrl Pts',(-0.132736616375526,0.0788581785466829,
1.2045621652883));
#14073=CARTESIAN_POINT('Ctrl Pts',(-0.143159994183491,0.0315270405159292,
1.20720955466256));
#14074=CARTESIAN_POINT('Ctrl Pts',(-0.145423823013163,0.021247302336111,
1.20778453491361));
#14075=CARTESIAN_POINT('Ctrl Pts',(-0.146470795531708,0.0106995851133921,
1.20835951516466));
#14076=CARTESIAN_POINT('Ctrl Pts',(-0.146373054956946,0.000132657382717961,
1.20893449541571));
#14077=CARTESIAN_POINT('Origin',(0.,0.,0.));
#14078=CARTESIAN_POINT('',(-0.146120596765396,-4.14129048147555E-5,1.26606550458429));
#14079=CARTESIAN_POINT('',(-0.146109918970638,-1.0198006988139E-5,1.25893449541571));
#14080=CARTESIAN_POINT('',(-0.14635,-1.79227059055215E-17,0.));
#14081=CARTESIAN_POINT('Ctrl Pts',(-0.146120596765396,-4.14129048147555E-5,
1.26606550458429));
#14082=CARTESIAN_POINT('Ctrl Pts',(-0.14605219935785,0.0269443530192317,
1.26460351894424));
#14083=CARTESIAN_POINT('Ctrl Pts',(-0.138898723445843,0.053963836666407,
1.26314153330418));
#14084=CARTESIAN_POINT('Ctrl Pts',(-0.124882896249422,0.0767650581554474,
1.26167954766413));
#14085=CARTESIAN_POINT('Ctrl Pts',(-0.0995129464537159,0.118037388097231,
1.25903321778503));
#14086=CARTESIAN_POINT('Ctrl Pts',(-0.051658938874944,0.145488850208621,
1.25638688790592));
#14087=CARTESIAN_POINT('Ctrl Pts',(-0.00322440565727106,0.146554478394238,
1.25374055802682));
#14088=CARTESIAN_POINT('Ctrl Pts',(0.0452101275604033,0.147620106579856,
1.25109422814772));
#14089=CARTESIAN_POINT('Ctrl Pts',(0.0942251864169787,0.122299900839699,
1.24844789826862));
#14090=CARTESIAN_POINT('Ctrl Pts',(0.121385807331354,0.0821833176976391,
1.24580156838952));
#14091=CARTESIAN_POINT('Ctrl Pts',(0.148546428245729,0.0420667345555804,
1.24315523851041));
#14092=CARTESIAN_POINT('Ctrl Pts',(0.153852611217905,-0.0128462259883804,
1.24050890863131));
#14093=CARTESIAN_POINT('Ctrl Pts',(0.134875632820701,-0.0574210379606392,
1.23786257875221));
#14094=CARTESIAN_POINT('Ctrl Pts',(0.115898654423498,-0.101995849932898,
1.23521624887311));
#14095=CARTESIAN_POINT('Ctrl Pts',(0.0726385146569148,-0.136232513333455,
1.23256991899401));
#14096=CARTESIAN_POINT('Ctrl Pts',(0.0248960600935515,-0.144460368686643,
1.2299235891149));
#14097=CARTESIAN_POINT('Ctrl Pts',(-0.0228463944698117,-0.152688224039831,
1.2272772592358));
#14098=CARTESIAN_POINT('Ctrl Pts',(-0.0750711638299551,-0.134907271345651,
1.2246309293567));
#14099=CARTESIAN_POINT('Ctrl Pts',(-0.107874149410843,-0.0992561323957017,
1.2219845994776));
#14100=CARTESIAN_POINT('Ctrl Pts',(-0.132331163880887,-0.072675612185966,
1.2200115678465));
#14101=CARTESIAN_POINT('Ctrl Pts',(-0.145992019903337,-0.0361614337449312,
1.21803853621539));
#14102=CARTESIAN_POINT('Ctrl Pts',(-0.146318311025392,0.000133437649768732,
1.21606550458429));
#14103=CARTESIAN_POINT('Ctrl Pts',(-0.146373054956946,0.000132657382717961,
1.20893449541571));
#14104=CARTESIAN_POINT('Ctrl Pts',(-0.146020767276673,-0.0379538636644633,
1.21100690453892));
#14105=CARTESIAN_POINT('Ctrl Pts',(-0.130797424420382,-0.0762899498869128,
1.21307931366213));
#14106=CARTESIAN_POINT('Ctrl Pts',(-0.104081054125652,-0.103227285106232,
1.21515172278534));
#14107=CARTESIAN_POINT('Ctrl Pts',(-0.0699523514264828,-0.137638258418326,
1.2177991121596));
#14108=CARTESIAN_POINT('Ctrl Pts',(-0.0170685611947798,-0.153447990763203,
1.22044650153386));
#14109=CARTESIAN_POINT('Ctrl Pts',(0.0303468241642401,-0.143414812629152,
1.22309389090812));
#14110=CARTESIAN_POINT('Ctrl Pts',(0.0777622095232573,-0.133381634495101,
1.22574128028238));
#14111=CARTESIAN_POINT('Ctrl Pts',(0.119709190009594,-0.0975055458821257,
1.22838866965664));
#14112=CARTESIAN_POINT('Ctrl Pts',(0.136973893871985,-0.052219638220276,
1.2310360590309));
#14113=CARTESIAN_POINT('Ctrl Pts',(0.154238597734379,-0.00693373055842239,
1.23368344840516));
#14114=CARTESIAN_POINT('Ctrl Pts',(0.146821024972825,0.0477619961523044,
1.23633083777942));
#14115=CARTESIAN_POINT('Ctrl Pts',(0.118118804930222,0.0868140895256425,
1.23897822715368));
#14116=CARTESIAN_POINT('Ctrl Pts',(0.0894165848876198,0.125866182898978,
1.24162561652794));
#14117=CARTESIAN_POINT('Ctrl Pts',(0.0394297175639698,0.149274642934924,
1.2442730059022));
#14118=CARTESIAN_POINT('Ctrl Pts',(-0.00894524413350711,0.146317192515786,
1.24692039527646));
#14119=CARTESIAN_POINT('Ctrl Pts',(-0.0573202058309854,0.143359742096648,
1.24956778465072));
#14120=CARTESIAN_POINT('Ctrl Pts',(-0.104083261902292,0.114036381222425,
1.25221517402498));
#14121=CARTESIAN_POINT('Ctrl Pts',(-0.127814530591109,0.0717787154251623,
1.25486256339924));
#14122=CARTESIAN_POINT('Ctrl Pts',(-0.139981499518435,0.0501133037087236,
1.2562198740714));
#14123=CARTESIAN_POINT('Ctrl Pts',(-0.146094355379323,0.0250479932723348,
1.25757718474355));
#14124=CARTESIAN_POINT('Ctrl Pts',(-0.146109918970638,-1.0198006988139E-5,
1.25893449541571));
#14125=CARTESIAN_POINT('Origin',(0.,0.,0.));
#14126=CARTESIAN_POINT('',(-0.146470135615938,-0.000111966546850736,1.31606550458429));
#14127=CARTESIAN_POINT('',(-0.146410535958061,-0.000127756381200432,1.30893449541571));
#14128=CARTESIAN_POINT('',(-0.14635,-1.79227059055215E-17,0.));
#14129=CARTESIAN_POINT('Ctrl Pts',(-0.146470135615938,-0.000111966546850736,
1.31606550458429));
#14130=CARTESIAN_POINT('Ctrl Pts',(-0.146120207411574,0.0411799307449602,
1.31381483155218));
#14131=CARTESIAN_POINT('Ctrl Pts',(-0.127827491572984,0.0827431563937987,
1.31156415852007));
#14132=CARTESIAN_POINT('Ctrl Pts',(-0.0969137672218927,0.10998333351997,
1.30931348548796));
#14133=CARTESIAN_POINT('Ctrl Pts',(-0.0605655677022408,0.142012194937238,
1.30666715560886));
#14134=CARTESIAN_POINT('Ctrl Pts',(-0.00676890401288169,0.154239532672684,
1.30402082572976));
#14135=CARTESIAN_POINT('Ctrl Pts',(0.0398526445220406,0.14106870189023,
1.30137449585066));
#14136=CARTESIAN_POINT('Ctrl Pts',(0.0864741930569617,0.127897871107775,
1.29872816597155));
#14137=CARTESIAN_POINT('Ctrl Pts',(0.125920626437448,0.0893288718074177,
1.29608183609245));
#14138=CARTESIAN_POINT('Ctrl Pts',(0.14013669149516,0.0430153417578024,
1.29343550621335));
#14139=CARTESIAN_POINT('Ctrl Pts',(0.154352756552873,-0.00329818829181684,
1.29078917633425));
#14140=CARTESIAN_POINT('Ctrl Pts',(0.143338453287813,-0.0573562490906975,
1.28814284645515));
#14141=CARTESIAN_POINT('Ctrl Pts',(0.112135201594409,-0.0944156157243562,
1.28549651657604));
#14142=CARTESIAN_POINT('Ctrl Pts',(0.0809319499010078,-0.131474982358013,
1.28285018669694));
#14143=CARTESIAN_POINT('Ctrl Pts',(0.0295397497792676,-0.151535654826449,
1.28020385681784));
#14144=CARTESIAN_POINT('Ctrl Pts',(-0.0185183802362589,-0.1454155477333,
1.27755752693874));
#14145=CARTESIAN_POINT('Ctrl Pts',(-0.066576510251784,-0.139295440640151,
1.27491119705964));
#14146=CARTESIAN_POINT('Ctrl Pts',(-0.111300570161094,-0.106994553985419,
1.27226486718053));
#14147=CARTESIAN_POINT('Ctrl Pts',(-0.13221965410943,-0.0632975117719662,
1.26961853730143));
#14148=CARTESIAN_POINT('Ctrl Pts',(-0.141581826511298,-0.0437412423069929,
1.26843419306239));
#14149=CARTESIAN_POINT('Ctrl Pts',(-0.146176005022067,-0.0219023912433209,
1.26724984882334));
#14150=CARTESIAN_POINT('Ctrl Pts',(-0.146120596765396,-4.14129048147555E-5,
1.26606550458429));
#14151=CARTESIAN_POINT('Ctrl Pts',(-0.146109918970638,-1.0198006988139E-5,
1.25893449541571));
#14152=CARTESIAN_POINT('Ctrl Pts',(-0.146124711647138,-0.0238271763493914,
1.26022457411781));
#14153=CARTESIAN_POINT('Ctrl Pts',(-0.140631289159497,-0.0476377233371588,
1.26151465281992));
#14154=CARTESIAN_POINT('Ctrl Pts',(-0.129592576141605,-0.0685164391025303,
1.26280473152202));
#14155=CARTESIAN_POINT('Ctrl Pts',(-0.106939871696956,-0.111361957112663,
1.26545212089628));
#14156=CARTESIAN_POINT('Ctrl Pts',(-0.0609349815013302,-0.141861022412626,
1.26809951027054));
#14157=CARTESIAN_POINT('Ctrl Pts',(-0.0126505083952331,-0.146043496451057,
1.2707468996448));
#14158=CARTESIAN_POINT('Ctrl Pts',(0.0356339647108625,-0.150225970489488,
1.27339428901906));
#14159=CARTESIAN_POINT('Ctrl Pts',(0.0861980207274291,-0.128091853266388,
1.27604167839332));
#14160=CARTESIAN_POINT('Ctrl Pts',(0.11588072467734,-0.0897797074320025,
1.27868906776758));
#14161=CARTESIAN_POINT('Ctrl Pts',(0.145563428627253,-0.0514675615976161,
1.28133645714184));
#14162=CARTESIAN_POINT('Ctrl Pts',(0.154364780510509,0.00302261284805656,
1.2839838465161));
#14163=CARTESIAN_POINT('Ctrl Pts',(0.138253309066183,0.0487315170146188,
1.28663123589036));
#14164=CARTESIAN_POINT('Ctrl Pts',(0.122141837621857,0.0944404211811797,
1.28927862526462));
#14165=CARTESIAN_POINT('Ctrl Pts',(0.0811175428499519,0.131368055068631,
1.29192601463888));
#14166=CARTESIAN_POINT('Ctrl Pts',(0.0339716590485425,0.142599665496764,
1.29457340401314));
#14167=CARTESIAN_POINT('Ctrl Pts',(-0.013174224752867,0.153831275924897,
1.2972207933874));
#14168=CARTESIAN_POINT('Ctrl Pts',(-0.0664416975837803,0.139366862893713,
1.29986818276166));
#14169=CARTESIAN_POINT('Ctrl Pts',(-0.101431520699135,0.105831870563862,
1.30251557213592));
#14170=CARTESIAN_POINT('Ctrl Pts',(-0.129710573305276,0.0787286237393239,
1.30465521322918));
#14171=CARTESIAN_POINT('Ctrl Pts',(-0.146050663974784,0.0391684733249047,
1.30679485432245));
#14172=CARTESIAN_POINT('Ctrl Pts',(-0.146410535958061,-0.000127756381200432,
1.30893449541571));
#14173=CARTESIAN_POINT('Origin',(0.,0.,0.));
#14174=CARTESIAN_POINT('',(-0.146471469669193,0.000111495080380188,1.36606550458429));
#14175=CARTESIAN_POINT('',(-0.146526884620975,8.5711493927648E-5,1.35893449541571));
#14176=CARTESIAN_POINT('',(-0.14635,-1.79227059055215E-17,0.));
#14177=CARTESIAN_POINT('Ctrl Pts',(-0.146471469669193,0.000111495080380188,
1.36606550458429));
#14178=CARTESIAN_POINT('Ctrl Pts',(-0.146532402405025,0.0073220458586883,
1.36567247403923));
#14179=CARTESIAN_POINT('Ctrl Pts',(-0.146045973070864,0.0145243451116175,
1.36527944349416));
#14180=CARTESIAN_POINT('Ctrl Pts',(-0.144983764805735,0.0216407019395156,
1.3648864129491));
#14181=CARTESIAN_POINT('Ctrl Pts',(-0.137831767320671,0.0695561322809842,
1.36224008307));
#14182=CARTESIAN_POINT('Ctrl Pts',(-0.104576727819841,0.113575347233418,
1.3595937531909));
#14183=CARTESIAN_POINT('Ctrl Pts',(-0.060440002550743,0.133550058215342,
1.3569474233118));
#14184=CARTESIAN_POINT('Ctrl Pts',(-0.0163032772816473,0.153524769197265,
1.35430109343269));
#14185=CARTESIAN_POINT('Ctrl Pts',(0.0387151337557165,0.149454976208681,
1.35165476355359));
#14186=CARTESIAN_POINT('Ctrl Pts',(0.0794324390145508,0.123203488242689,
1.34900843367449));
#14187=CARTESIAN_POINT('Ctrl Pts',(0.120149744273387,0.0969520002766962,
1.34636210379539));
#14188=CARTESIAN_POINT('Ctrl Pts',(0.146565943753694,0.048518817333291,
1.34371577391629));
#14189=CARTESIAN_POINT('Ctrl Pts',(0.14658992694451,7.25688577880009E-5,
1.34106944403718));
#14190=CARTESIAN_POINT('Ctrl Pts',(0.146613910135327,-0.0483736796177136,
1.33842311415808));
#14191=CARTESIAN_POINT('Ctrl Pts',(0.120245677036657,-0.0968329936253116,
1.33577678427898));
#14192=CARTESIAN_POINT('Ctrl Pts',(0.0795543829983497,-0.123124782547022,
1.33313045439988));
#14193=CARTESIAN_POINT('Ctrl Pts',(0.0388630889600415,-0.149416571468734,
1.33048412452078));
#14194=CARTESIAN_POINT('Ctrl Pts',(-0.0161512660179049,-0.153540835304554,
1.32783779464168));
#14195=CARTESIAN_POINT('Ctrl Pts',(-0.0603077462478081,-0.133609833714981,
1.32519146476257));
#14196=CARTESIAN_POINT('Ctrl Pts',(-0.10446422647771,-0.113678832125408,
1.32254513488347));
#14197=CARTESIAN_POINT('Ctrl Pts',(-0.137762831959571,-0.0696925651104417,
1.31989880500437));
#14198=CARTESIAN_POINT('Ctrl Pts',(-0.144962267025529,-0.0217842390534145,
1.31725247512527));
#14199=CARTESIAN_POINT('Ctrl Pts',(-0.146038665626028,-0.0146213916011371,
1.31685681827827));
#14200=CARTESIAN_POINT('Ctrl Pts',(-0.146531651210624,-0.00737087161912708,
1.31646116143128));
#14201=CARTESIAN_POINT('Ctrl Pts',(-0.146470135615938,-0.000111966546850736,
1.31606550458429));
#14202=CARTESIAN_POINT('Ctrl Pts',(-0.146410535958061,-0.000127756381200432,
1.30893449541571));
#14203=CARTESIAN_POINT('Ctrl Pts',(-0.146495935505426,-0.00945296197092968,
1.30944224369671));
#14204=CARTESIAN_POINT('Ctrl Pts',(-0.145681427739287,-0.018763305174839,
1.3099499919777));
#14205=CARTESIAN_POINT('Ctrl Pts',(-0.143913007029536,-0.0278887903271487,
1.3104577402587));
#14206=CARTESIAN_POINT('Ctrl Pts',(-0.134692496844786,-0.0754688872597875,
1.31310512963296));
#14207=CARTESIAN_POINT('Ctrl Pts',(-0.0995393030754929,-0.118023509496548,
1.31575251900722));
#14208=CARTESIAN_POINT('Ctrl Pts',(-0.0545553941775042,-0.136060454153345,
1.31839990838148));
#14209=CARTESIAN_POINT('Ctrl Pts',(-0.00957148527951295,-0.154097398810142,
1.32104729775574));
#14210=CARTESIAN_POINT('Ctrl Pts',(0.0452431387471776,-0.14761666588697,
1.32369468713));
#14211=CARTESIAN_POINT('Ctrl Pts',(0.0847805644327026,-0.119586763955155,
1.32634207650426));
#14212=CARTESIAN_POINT('Ctrl Pts',(0.124317990118227,-0.09155686202334,
1.32898946587852));
#14213=CARTESIAN_POINT('Ctrl Pts',(0.148578217462589,-0.041977791082884,
1.33163685525278));
#14214=CARTESIAN_POINT('Ctrl Pts',(0.146448816178573,0.00644068764408242,
1.33428424462704));
#14215=CARTESIAN_POINT('Ctrl Pts',(0.144319414894557,0.0548591663710502,
1.3369316340013));
#14216=CARTESIAN_POINT('Ctrl Pts',(0.115800384982161,0.102117052884526,
1.33957902337556));
#14217=CARTESIAN_POINT('Ctrl Pts',(0.0739549070570988,0.126567807678519,
1.34222641274982));
#14218=CARTESIAN_POINT('Ctrl Pts',(0.0321094291320376,0.151018562472512,
1.34487380212408));
#14219=CARTESIAN_POINT('Ctrl Pts',(-0.0230624968056921,0.152662185547021,
1.34752119149834));
#14220=CARTESIAN_POINT('Ctrl Pts',(-0.0662892946253695,0.1307458130856,
1.3501685808726));
#14221=CARTESIAN_POINT('Ctrl Pts',(-0.109516092445046,0.10882944062418,
1.35281597024686));
#14222=CARTESIAN_POINT('Ctrl Pts',(-0.140797762146673,0.0633530726268328,
1.35546335962112));
#14223=CARTESIAN_POINT('Ctrl Pts',(-0.145805692234247,0.0151472216574969,
1.35811074899538));
#14224=CARTESIAN_POINT('Ctrl Pts',(-0.146325105122407,0.0101474034011793,
1.35838533113549));
#14225=CARTESIAN_POINT('Ctrl Pts',(-0.146561879835735,0.00511822289583405,
1.3586599132756));
#14226=CARTESIAN_POINT('Ctrl Pts',(-0.146526884620975,8.5711493927648E-5,
1.35893449541571));
#14227=CARTESIAN_POINT('Origin',(0.,0.,0.));
#14228=CARTESIAN_POINT('',(-0.146120987371435,4.2191387702159E-5,1.41606550458429));
#14229=CARTESIAN_POINT('',(-0.146148882937928,7.6306569664006E-5,1.40893449541571));
#14230=CARTESIAN_POINT('',(-0.14635,-1.79227059055215E-17,0.));
#14231=CARTESIAN_POINT('Ctrl Pts',(-0.146120987371435,4.2191387702159E-5,
1.41606550458429));
#14232=CARTESIAN_POINT('Ctrl Pts',(-0.146177309023295,0.021854523983563,
1.41488378664717));
#14233=CARTESIAN_POINT('Ctrl Pts',(-0.141604359564088,0.0436444172696427,
1.41370206871005));
#14234=CARTESIAN_POINT('Ctrl Pts',(-0.132282279973341,0.0631665524487371,
1.41252035077294));
#14235=CARTESIAN_POINT('Ctrl Pts',(-0.1114064880593,0.106884268839086,1.40987402089383));
#14236=CARTESIAN_POINT('Ctrl Pts',(-0.0667143915920224,0.139229456738304,
1.40722769101473));
#14237=CARTESIAN_POINT('Ctrl Pts',(-0.0186623352932378,0.145397151366753,
1.40458136113563));
#14238=CARTESIAN_POINT('Ctrl Pts',(0.0293897210055454,0.151564845995202,
1.40193503125653));
#14239=CARTESIAN_POINT('Ctrl Pts',(0.0808017371358351,0.131555047352884,
1.39928870137743));
#14240=CARTESIAN_POINT('Ctrl Pts',(0.112041660826149,0.0945265884816804,
1.39664237149832));
#14241=CARTESIAN_POINT('Ctrl Pts',(0.143281584516463,0.0574981296104763,
1.39399604161922));
#14242=CARTESIAN_POINT('Ctrl Pts',(0.154349415766802,0.00345101051038574,
1.39134971174012));
#14243=CARTESIAN_POINT('Ctrl Pts',(0.140179214932283,-0.0428765696854336,
1.38870338186102));
#14244=CARTESIAN_POINT('Ctrl Pts',(0.126009014097764,-0.089204149881253,
1.38605705198192));
#14245=CARTESIAN_POINT('Ctrl Pts',(0.0866007811783877,-0.127812191172801,
1.38341072210282));
#14246=CARTESIAN_POINT('Ctrl Pts',(0.0399922944706322,-0.14102917638501,
1.38076439222371));
#14247=CARTESIAN_POINT('Ctrl Pts',(-0.00661619223712474,-0.15424616159722,
1.37811806234461));
#14248=CARTESIAN_POINT('Ctrl Pts',(-0.060424932733261,-0.142072090730089,
1.37547173246551));
#14249=CARTESIAN_POINT('Ctrl Pts',(-0.0968048252466797,-0.110079232431271,
1.37282540258641));
#14250=CARTESIAN_POINT('Ctrl Pts',(-0.127781608685608,-0.08283792481198,
1.37057210325237));
#14251=CARTESIAN_POINT('Ctrl Pts',(-0.146122133733866,-0.0412276055847571,
1.36831880391833));
#14252=CARTESIAN_POINT('Ctrl Pts',(-0.146471469669193,0.000111495080380188,
1.36606550458429));
#14253=CARTESIAN_POINT('Ctrl Pts',(-0.146526884620975,8.5711493927648E-5,
1.35893449541571));
#14254=CARTESIAN_POINT('Ctrl Pts',(-0.146224472749943,-0.0434028397118431,
1.36130730264986));
#14255=CARTESIAN_POINT('Ctrl Pts',(-0.125627402569456,-0.0871401285467012,
1.36368010988401));
#14256=CARTESIAN_POINT('Ctrl Pts',(-0.0917490966422633,-0.114327780902106,
1.36605291711816));
#14257=CARTESIAN_POINT('Ctrl Pts',(-0.0539503804891888,-0.144661598551044,
1.36870030649242));
#14258=CARTESIAN_POINT('Ctrl Pts',(0.00038124229047478,-0.154393899907594,
1.37134769586668));
#14259=CARTESIAN_POINT('Ctrl Pts',(0.0463590973565905,-0.139066790892088,
1.37399508524094));
#14260=CARTESIAN_POINT('Ctrl Pts',(0.0923369524227062,-0.123739681876581,
1.3766424746152));
#14261=CARTESIAN_POINT('Ctrl Pts',(0.129961039775272,-0.083353162489017,
1.37928986398946));
#14262=CARTESIAN_POINT('Ctrl Pts',(0.141997595260484,-0.0364063334065561,
1.38193725336372));
#14263=CARTESIAN_POINT('Ctrl Pts',(0.154034150745695,0.0105404956759021,
1.38458464273798));
#14264=CARTESIAN_POINT('Ctrl Pts',(0.140483174363557,0.0640476344532581,
1.38723203211224));
#14265=CARTESIAN_POINT('Ctrl Pts',(0.10755170844225,0.0996060653705087,
1.3898794214865));
#14266=CARTESIAN_POINT('Ctrl Pts',(0.0746202425209409,0.135164496287762,
1.39252681086076));
#14267=CARTESIAN_POINT('Ctrl Pts',(0.0223082870604623,0.152774219344908,
1.39517420023502));
#14268=CARTESIAN_POINT('Ctrl Pts',(-0.025422593472234,0.144369075867769,
1.39782158960928));
#14269=CARTESIAN_POINT('Ctrl Pts',(-0.073153474004929,0.135963932390631,
1.40046897898354));
#14270=CARTESIAN_POINT('Ctrl Pts',(-0.11630327960984,0.101543922379208,
1.4031163683578));
#14271=CARTESIAN_POINT('Ctrl Pts',(-0.135107186188192,0.0568751802851974,
1.40576375773206));
#14272=CARTESIAN_POINT('Ctrl Pts',(-0.142614236437708,0.0390421576584788,
1.40682067029328));
#14273=CARTESIAN_POINT('Ctrl Pts',(-0.14624095998336,0.0195756595648056,
1.40787758285449));
#14274=CARTESIAN_POINT('Ctrl Pts',(-0.146148882937928,7.6306569664006E-5,
1.40893449541571));
#14275=CARTESIAN_POINT('Origin',(0.,0.,0.));
#14276=CARTESIAN_POINT('',(-0.14631473222987,-0.000131398079681141,1.46606550458429));
#14277=CARTESIAN_POINT('',(-0.146248097568756,-0.000123763188177425,1.45893449541571));
#14278=CARTESIAN_POINT('',(-0.14635,-1.79227059055215E-17,0.));
#14279=CARTESIAN_POINT('Ctrl Pts',(-0.14631473222987,-0.000131398079681141,
1.46606550458429));
#14280=CARTESIAN_POINT('Ctrl Pts',(-0.145989697979493,0.0361157155227289,
1.46409509925512));
#14281=CARTESIAN_POINT('Ctrl Pts',(-0.132370868650209,0.0725796635271419,
1.46212469392594));
#14282=CARTESIAN_POINT('Ctrl Pts',(-0.107973319296019,0.0991484059484618,
1.46015428859677));
#14283=CARTESIAN_POINT('Ctrl Pts',(-0.0752064754000165,0.134831245351468,
1.45750795871767));
#14284=CARTESIAN_POINT('Ctrl Pts',(-0.0229974942306327,0.152665588379184,
1.45486162883857));
#14285=CARTESIAN_POINT('Ctrl Pts',(0.0247535192036911,0.144485406820094,
1.45221529895946));
#14286=CARTESIAN_POINT('Ctrl Pts',(0.0725045326380122,0.136305225261004,
1.44956896908036));
#14287=CARTESIAN_POINT('Ctrl Pts',(0.115797578337275,0.102110519115111,
1.44692263920126));
#14288=CARTESIAN_POINT('Ctrl Pts',(0.134818450998255,0.0575543070937695,
1.44427630932216));
#14289=CARTESIAN_POINT('Ctrl Pts',(0.153839323659235,0.0129980950724284,
1.44162997944306));
#14290=CARTESIAN_POINT('Ctrl Pts',(0.148588023281934,-0.0419196228243577,
1.43898364956396));
#14291=CARTESIAN_POINT('Ctrl Pts',(0.121467255745355,-0.082062966762292,
1.43633731968485));
#14292=CARTESIAN_POINT('Ctrl Pts',(0.0943464882087764,-0.122206310700226,
1.43369098980575));
#14293=CARTESIAN_POINT('Ctrl Pts',(0.0453562535129183,-0.147575280679306,
1.43104465992665));
#14294=CARTESIAN_POINT('Ctrl Pts',(-0.00307937473935208,-0.146557666176543,
1.42839833004755));
#14295=CARTESIAN_POINT('Ctrl Pts',(-0.0515150029916225,-0.14554005167378,
1.42575200016845));
#14296=CARTESIAN_POINT('Ctrl Pts',(-0.0993960248003067,-0.118135852689175,
1.42310567028934));
#14297=CARTESIAN_POINT('Ctrl Pts',(-0.124806792024246,-0.0768886307561326,
1.42045934041024));
#14298=CARTESIAN_POINT('Ctrl Pts',(-0.138870387581649,-0.0540603453281256,
1.41899472846826));
#14299=CARTESIAN_POINT('Ctrl Pts',(-0.146051182757901,-0.0269918425378075,
1.41753011652627));
#14300=CARTESIAN_POINT('Ctrl Pts',(-0.146120987371435,4.2191387702159E-5,
1.41606550458429));
#14301=CARTESIAN_POINT('Ctrl Pts',(-0.146148882937928,7.6306569664006E-5,
1.40893449541571));
#14302=CARTESIAN_POINT('Ctrl Pts',(-0.146010322369016,-0.0292669616874671,
1.41052497222875));
#14303=CARTESIAN_POINT('Ctrl Pts',(-0.137450455640384,-0.0586846305953837,
1.4121154490418));
#14304=CARTESIAN_POINT('Ctrl Pts',(-0.121019719714466,-0.0827222215753489,
1.41370592585484));
#14305=CARTESIAN_POINT('Ctrl Pts',(-0.0936703391105966,-0.122733407165291,
1.4163533152291));
#14306=CARTESIAN_POINT('Ctrl Pts',(-0.0445135703510636,-0.147838304168576,
1.41900070460336));
#14307=CARTESIAN_POINT('Ctrl Pts',(0.00393424939099551,-0.146537573651384,
1.42164809397762));
#14308=CARTESIAN_POINT('Ctrl Pts',(0.0523820691330518,-0.145236843134192,
1.42429548335188));
#14309=CARTESIAN_POINT('Ctrl Pts',(0.100120939857634,-0.117530485096527,
1.42694287272614));
#14310=CARTESIAN_POINT('Ctrl Pts',(0.125284029446909,-0.0761094471358441,
1.4295902621004));
#14311=CARTESIAN_POINT('Ctrl Pts',(0.150447119036187,-0.0346884091751576,
1.43223765147466));
#14312=CARTESIAN_POINT('Ctrl Pts',(0.153034427490153,0.020447308708549,
1.43488504084892));
#14313=CARTESIAN_POINT('Ctrl Pts',(0.13186079120536,0.0640427391611241,
1.43753243022318));
#14314=CARTESIAN_POINT('Ctrl Pts',(0.110687154920568,0.107638169613697,
1.44017981959744));
#14315=CARTESIAN_POINT('Ctrl Pts',(0.0657525738970213,0.139693312635139,
1.4428272089717));
#14316=CARTESIAN_POINT('Ctrl Pts',(0.0176394768514684,0.145525221357757,
1.44547459834596));
#14317=CARTESIAN_POINT('Ctrl Pts',(-0.0304736201940859,0.151357130080375,
1.44812198772022));
#14318=CARTESIAN_POINT('Ctrl Pts',(-0.0817652332616461,0.130965804504167,
1.45076937709448));
#14319=CARTESIAN_POINT('Ctrl Pts',(-0.112741325423428,0.0936916042199666,
1.45341676646874));
#14320=CARTESIAN_POINT('Ctrl Pts',(-0.134261605244105,0.0677957870194472,
1.45525600945106));
#14321=CARTESIAN_POINT('Ctrl Pts',(-0.145976367207401,0.0337512577971725,
1.45709525243339));
#14322=CARTESIAN_POINT('Ctrl Pts',(-0.146248097568756,-0.000123763188177425,
1.45893449541571));
#14323=CARTESIAN_POINT('Origin',(0.,0.,-0.0924367114736175));
#14324=CARTESIAN_POINT('',(-0.117746618301147,-0.000105742458702955,1.48256328852638));
#14325=CARTESIAN_POINT('',(-0.117971241274414,-5.28325160115065E-6,1.49243671147361));
#14326=CARTESIAN_POINT('',(-0.117775,2.85464118895969E-14,-0.0924367114736175));
#14327=CARTESIAN_POINT('',(-0.117668597464313,0.00500517689812599,1.532225));
#14328=CARTESIAN_POINT('Ctrl Pts',(-0.117746618301147,-0.000105742458702949,
1.48256328852638));
#14329=CARTESIAN_POINT('Ctrl Pts',(-0.117836347163251,-0.0101121102621826,
1.48323921307631));
#14330=CARTESIAN_POINT('Ctrl Pts',(-0.112089674709738,-0.0591937430214443,
1.48656146750534));
#14331=CARTESIAN_POINT('Ctrl Pts',(-0.0435804807853106,-0.132222740314769,
1.49253005181348));
#14332=CARTESIAN_POINT('Ctrl Pts',(0.0874774386997331,-0.108286040948335,
1.50046904145078));
#14333=CARTESIAN_POINT('Ctrl Pts',(0.138385550162814,0.0147146982980264,
1.50840803108809));
#14334=CARTESIAN_POINT('Ctrl Pts',(0.0627460642121078,0.124368470664037,
1.51634702072539));
#14335=CARTESIAN_POINT('Ctrl Pts',(-0.0706026869052757,0.119928391791904,
1.5242860103627));
#14336=CARTESIAN_POINT('Ctrl Pts',(-0.116004137797729,0.0441355889673283,
1.5295786701209));
#14337=CARTESIAN_POINT('Ctrl Pts',(-0.117668597464313,0.00500517689812487,
1.532225));
#14338=CARTESIAN_POINT('',(-0.0334019664627544,0.1129391839063,1.53222500000001));
#14339=CARTESIAN_POINT('Origin',(0.,0.,1.532225));
#14340=CARTESIAN_POINT('Ctrl Pts',(-0.117971276761593,-5.28420699491729E-6,
1.49243671147361));
#14341=CARTESIAN_POINT('Ctrl Pts',(-0.117971582784674,-0.000385634193345565,
1.49246252744444));
#14342=CARTESIAN_POINT('Ctrl Pts',(-0.117794795258817,-0.0397700451254522,
1.49513573278954));
#14343=CARTESIAN_POINT('Ctrl Pts',(-0.0742871760264013,-0.117748889605885,
1.50045632750888));
#14344=CARTESIAN_POINT('Ctrl Pts',(0.0586284551779338,-0.126233948370975,
1.50839849563167));
#14345=CARTESIAN_POINT('Ctrl Pts',(0.137995068118234,-0.019163470063063,
1.51634066375444));
#14346=CARTESIAN_POINT('Ctrl Pts',(0.0906261803825392,0.105639137646141,
1.52428283187723));
#14347=CARTESIAN_POINT('Ctrl Pts',(0.00417072711528833,0.124051375507138,
1.52957761062575));
#14348=CARTESIAN_POINT('Ctrl Pts',(-0.0334019664627544,0.1129391839063,
1.53222500000001));
#14349=CARTESIAN_POINT('Origin',(0.,0.,-0.0924367114736175));
#14350=CARTESIAN_POINT('',(-0.117590702341447,3.3953472435133E-5,1.43256328852638));
#14351=CARTESIAN_POINT('',(-0.117692994131604,-9.95982882293356E-5,1.44243671147361));
#14352=CARTESIAN_POINT('',(-0.117775,2.85464118895969E-14,-0.0924367114736175));
#14353=CARTESIAN_POINT('Ctrl Pts',(-0.117590702341447,3.39534724351446E-5,
1.43256328852638));
#14354=CARTESIAN_POINT('Ctrl Pts',(-0.117534527156218,-0.0217216553118358,
1.43402790046837));
#14355=CARTESIAN_POINT('Ctrl Pts',(-0.101314495966545,-0.0828641818343832,
1.43813884228945));
#14356=CARTESIAN_POINT('Ctrl Pts',(-0.00292444232197888,-0.139176693688359,
1.44489611398964));
#14357=CARTESIAN_POINT('Ctrl Pts',(0.115350068603298,-0.0779297424218237,
1.45283510362695));
#14358=CARTESIAN_POINT('Ctrl Pts',(0.128028003046829,0.0546551750765237,
1.46077409326425));
#14359=CARTESIAN_POINT('Ctrl Pts',(0.0235079116789307,0.137209630484779,
1.46871308290156));
#14360=CARTESIAN_POINT('Ctrl Pts',(-0.0918059616614023,0.0978189523496558,
1.47597614798894));
#14361=CARTESIAN_POINT('Ctrl Pts',(-0.117485047349053,0.0290640819657798,
1.48059288319721));
#14362=CARTESIAN_POINT('Ctrl Pts',(-0.117746618301147,-0.000105742458702949,
1.48256328852638));
#14363=CARTESIAN_POINT('Ctrl Pts',(-0.117692994131604,-9.9598288229346E-5,
1.44243671147361));
#14364=CARTESIAN_POINT('Ctrl Pts',(-0.117789077779518,-0.0120777797952868,
1.44324485786555));
#14365=CARTESIAN_POINT('Ctrl Pts',(-0.110597905189529,-0.0631824179582176,
1.44670039363175));
#14366=CARTESIAN_POINT('Ctrl Pts',(-0.0368790902657646,-0.134252921254984,
1.45280331877221));
#14367=CARTESIAN_POINT('Ctrl Pts',(0.0928396680879532,-0.103751556080299,
1.46074548689499));
#14368=CARTESIAN_POINT('Ctrl Pts',(0.137511141307062,0.0217950526079239,
1.46868765501776));
#14369=CARTESIAN_POINT('Ctrl Pts',(0.0562018483347667,0.127378648737854,
1.47662982314055));
#14370=CARTESIAN_POINT('Ctrl Pts',(-0.0761502833827582,0.1162998103107,
1.48454617529249));
#14371=CARTESIAN_POINT('Ctrl Pts',(-0.117940200573233,0.0386186906477724,
1.48981513807018));
#14372=CARTESIAN_POINT('Ctrl Pts',(-0.117971276761593,-5.28420699491729E-6,
1.49243671147361));
#14373=CARTESIAN_POINT('Origin',(0.,0.,-0.0924367114736175));
#14374=CARTESIAN_POINT('',(-0.117872752581409,8.97255421561373E-5,1.38256328852638));
#14375=CARTESIAN_POINT('',(-0.117613151267609,6.14076272390171E-5,1.39243671147361));
#14376=CARTESIAN_POINT('',(-0.117775,2.85464118895969E-14,-0.0924367114736175));
#14377=CARTESIAN_POINT('Ctrl Pts',(-0.117872752581409,8.97255421561322E-5,
1.38256328852638));
#14378=CARTESIAN_POINT('Ctrl Pts',(-0.117591624875346,-0.0331778698171688,
1.38481658786042));
#14379=CARTESIAN_POINT('Ctrl Pts',(-0.0854981695600773,-0.105990339321694,
1.38971621707357));
#14380=CARTESIAN_POINT('Ctrl Pts',(0.0379781508110965,-0.133926497290667,
1.39726217616581));
#14381=CARTESIAN_POINT('Ctrl Pts',(0.133119345865688,-0.0407171622080862,
1.40520116580311));
#14382=CARTESIAN_POINT('Ctrl Pts',(0.106398871137127,0.0897659150453452,
1.41314015544042));
#14383=CARTESIAN_POINT('Ctrl Pts',(-0.0177224175491345,0.138074504763813,
1.42107914507772));
#14384=CARTESIAN_POINT('Ctrl Pts',(-0.105714817800915,0.0743914165933911,
1.42755352277305));
#14385=CARTESIAN_POINT('Ctrl Pts',(-0.11763602712824,0.0175874039095825,
1.43138157058926));
#14386=CARTESIAN_POINT('Ctrl Pts',(-0.117590702341447,3.39534724351446E-5,
1.43256328852638));
#14387=CARTESIAN_POINT('Ctrl Pts',(-0.117613151267609,6.1407627239024E-5,
1.39243671147361));
#14388=CARTESIAN_POINT('Ctrl Pts',(-0.117501644803633,-0.0235525549213426,
1.39402718828666));
#14389=CARTESIAN_POINT('Ctrl Pts',(-0.0991469449676741,-0.0866320980727062,
1.39826505447396));
#14390=CARTESIAN_POINT('Ctrl Pts',(0.00373660876362508,-0.139175849115243,
1.40515031003553));
#14391=CARTESIAN_POINT('Ctrl Pts',(0.118990018389619,-0.0722858665142316,
1.41309247815831));
#14392=CARTESIAN_POINT('Ctrl Pts',(0.125236419206141,0.0608253567263532,
1.42103464628109));
#14393=CARTESIAN_POINT('Ctrl Pts',(0.0167532566496359,0.13821437898841,
1.42897681440387));
#14394=CARTESIAN_POINT('Ctrl Pts',(-0.0944771051913143,0.0939940009069027,
1.43611083613471));
#14395=CARTESIAN_POINT('Ctrl Pts',(-0.117474319425011,0.0271612872365273,
1.44059746849129));
#14396=CARTESIAN_POINT('Ctrl Pts',(-0.117692994131604,-9.9598288229346E-5,
1.44243671147361));
#14397=CARTESIAN_POINT('Origin',(0.,0.,-0.0924367114736175));
#14398=CARTESIAN_POINT('',(-0.117871679003533,-9.01049542302267E-5,1.33256328852638));
#14399=CARTESIAN_POINT('',(-0.117917347702326,6.89762296073142E-5,1.34243671147361));
#14400=CARTESIAN_POINT('',(-0.117775,2.85464118895969E-14,-0.0924367114736175));
#14401=CARTESIAN_POINT('Ctrl Pts',(-0.117871679003533,-9.01049542302501E-5,
1.33256328852638));
#14402=CARTESIAN_POINT('Ctrl Pts',(-0.117921183610054,-0.00593170075121234,
1.33295894537338));
#14403=CARTESIAN_POINT('Ctrl Pts',(-0.114870949065289,-0.0507926200311143,
1.33600093209947));
#14404=CARTESIAN_POINT('Ctrl Pts',(-0.0572704544775333,-0.126880813469472,
1.34168924870467));
#14405=CARTESIAN_POINT('Ctrl Pts',(0.0755477687720905,-0.116923823242002,
1.34962823834197));
#14406=CARTESIAN_POINT('Ctrl Pts',(0.13920718769651,6.89141801743488E-5,
1.35756722797928));
#14407=CARTESIAN_POINT('Ctrl Pts',(0.0754319660950179,0.116998564767658,
1.36550621761658));
#14408=CARTESIAN_POINT('Ctrl Pts',(-0.0573960494825499,0.126824048933643,
1.37344520725389));
#14409=CARTESIAN_POINT('Ctrl Pts',(-0.11489462347839,0.0507140179075799,
1.37913089755716));
#14410=CARTESIAN_POINT('Ctrl Pts',(-0.117921788132912,0.00589240827474643,
1.38217025798132));
#14411=CARTESIAN_POINT('Ctrl Pts',(-0.117872752581409,8.97255421561322E-5,
1.38256328852638));
#14412=CARTESIAN_POINT('Ctrl Pts',(-0.117917347702326,6.89762296073276E-5,
1.34243671147361));
#14413=CARTESIAN_POINT('Ctrl Pts',(-0.117673982084908,-0.0349283870656527,
1.34480951870776));
#14414=CARTESIAN_POINT('Ctrl Pts',(-0.0826049238592893,-0.109396528181867,
1.34982971531618));
#14415=CARTESIAN_POINT('Ctrl Pts',(0.0440301174146577,-0.132080378229483,
1.35749730129884));
#14416=CARTESIAN_POINT('Ctrl Pts',(0.13486394497766,-0.0345773583278084,
1.36543946942163));
#14417=CARTESIAN_POINT('Ctrl Pts',(0.102148545386143,0.0946020732301706,
1.3733816375444));
#14418=CARTESIAN_POINT('Ctrl Pts',(-0.0241454188302812,0.137116288461919,
1.38132380566719));
#14419=CARTESIAN_POINT('Ctrl Pts',(-0.107458038693719,0.07065895059964,
1.38767549697692));
#14420=CARTESIAN_POINT('Ctrl Pts',(-0.117687250167678,0.015753490298928,
1.3913797989124));
#14421=CARTESIAN_POINT('Ctrl Pts',(-0.117613151267609,6.1407627239024E-5,
1.39243671147361));
#14422=CARTESIAN_POINT('Origin',(0.,0.,-0.0924367114736175));
#14423=CARTESIAN_POINT('',(-0.117590388001671,-3.33269891443968E-5,1.28256328852638));
#14424=CARTESIAN_POINT('',(-0.117823716245033,-0.000102811805890834,1.29243671147362));
#14425=CARTESIAN_POINT('',(-0.117775,2.85464118895969E-14,-0.0924367114736175));
#14426=CARTESIAN_POINT('Ctrl Pts',(-0.117590388001671,-3.33269891444124E-5,
1.28256328852638));
#14427=CARTESIAN_POINT('Ctrl Pts',(-0.117634977734708,-0.017625925033684,
1.28374763276543));
#14428=CARTESIAN_POINT('Ctrl Pts',(-0.105676786131388,-0.0744702911817869,
1.28757830688358));
#14429=CARTESIAN_POINT('Ctrl Pts',(-0.0175857351491984,-0.138091953858251,
1.29405531088083));
#14430=CARTESIAN_POINT('Ctrl Pts',(0.106487712804436,-0.089660542174548,
1.30199430051814));
#14431=CARTESIAN_POINT('Ctrl Pts',(0.133078957772855,0.0408489510387311,
1.30993329015544));
#14432=CARTESIAN_POINT('Ctrl Pts',(0.0378455373822902,0.133964029124136,
1.31787227979275));
#14433=CARTESIAN_POINT('Ctrl Pts',(-0.0855601048685178,0.105915403748908,
1.32541561258306));
#14434=CARTESIAN_POINT('Ctrl Pts',(-0.117590074669608,0.0331395035428114,
1.33031261549427));
#14435=CARTESIAN_POINT('Ctrl Pts',(-0.117871679003533,-9.01049542302501E-5,
1.33256328852638));
#14436=CARTESIAN_POINT('Ctrl Pts',(-0.117823716245033,-0.000102811805890825,
1.29243671147362));
#14437=CARTESIAN_POINT('Ctrl Pts',(-0.117892441435953,-0.00760726064997237,
1.29294445975461));
#14438=CARTESIAN_POINT('Ctrl Pts',(-0.113819337750002,-0.0541654333254181,
1.29609959740987));
#14439=CARTESIAN_POINT('Ctrl Pts',(-0.0518146499729274,-0.129225073214149,
1.30190212443939));
#14440=CARTESIAN_POINT('Ctrl Pts',(0.0805213734929343,-0.11357898534207,
1.30984429256217));
#14441=CARTESIAN_POINT('Ctrl Pts',(0.1390915465469,0.0061171215252809,1.31778646068495));
#14442=CARTESIAN_POINT('Ctrl Pts',(0.0702395735793815,0.120209316621791,
1.32572862880773));
#14443=CARTESIAN_POINT('Ctrl Pts',(-0.0629590648350173,0.124177428154433,
1.33367079693051));
#14444=CARTESIAN_POINT('Ctrl Pts',(-0.115917830154768,0.0471875384414626,
1.33924015781913));
#14445=CARTESIAN_POINT('Ctrl Pts',(-0.117945510062545,0.00411888419242175,
1.3421621293335));
#14446=CARTESIAN_POINT('Ctrl Pts',(-0.117917347702326,6.89762296073276E-5,
1.34243671147361));
#14447=CARTESIAN_POINT('Origin',(0.,0.,-0.0924367114736175));
#14448=CARTESIAN_POINT('',(-0.11774949833287,0.000107383800510985,1.23256328852638));
#14449=CARTESIAN_POINT('',(-0.117581795058195,-8.20683476789735E-6,1.24243671147361));
#14450=CARTESIAN_POINT('',(-0.117775,2.85464118895969E-14,-0.0924367114736175));
#14451=CARTESIAN_POINT('Ctrl Pts',(-0.11774949833287,0.000107383800510997,
1.23256328852638));
#14452=CARTESIAN_POINT('Ctrl Pts',(-0.1174869159147,-0.0291008736543001,
1.23453632015749));
#14453=CARTESIAN_POINT('Ctrl Pts',(-0.0917482398636095,-0.0978979247776974,
1.23915568166769));
#14454=CARTESIAN_POINT('Ctrl Pts',(0.0236422145726536,-0.137184880695923,
1.246421373057));
#14455=CARTESIAN_POINT('Ctrl Pts',(0.128082862902196,-0.0545291301253663,
1.2543603626943));
#14456=CARTESIAN_POINT('Ctrl Pts',(0.115272428336817,0.0780443019497631,
1.26229935233161));
#14457=CARTESIAN_POINT('Ctrl Pts',(-0.00306201423577413,0.139173524314926,
1.27023834196891));
#14458=CARTESIAN_POINT('Ctrl Pts',(-0.101358337705897,0.08278581645186,
1.27699298736717));
#14459=CARTESIAN_POINT('Ctrl Pts',(-0.117535345263889,0.02168343817453,
1.28110130288633));
#14460=CARTESIAN_POINT('Ctrl Pts',(-0.117590388001671,-3.33269891444124E-5,
1.28256328852638));
#14461=CARTESIAN_POINT('Ctrl Pts',(-0.117581795058195,-8.20683476789562E-6,
1.24243671147361));
#14462=CARTESIAN_POINT('Ctrl Pts',(-0.117593699448189,-0.0191748937105988,
1.24372679017572));
#14463=CARTESIAN_POINT('Ctrl Pts',(-0.104100832827715,-0.0776580224685839,
1.24766425825208));
#14464=CARTESIAN_POINT('Ctrl Pts',(-0.0120149744006178,-0.138706589206355,
1.25424911570271));
#14465=CARTESIAN_POINT('Ctrl Pts',(0.110059129405696,-0.0852693704304675,
1.26219128382548));
#14466=CARTESIAN_POINT('Ctrl Pts',(0.13130776387206,0.0462833517151888,
1.27013345194827));
#14467=CARTESIAN_POINT('Ctrl Pts',(0.0322649968732001,0.135435768819968,
1.27807562007105));
#14468=CARTESIAN_POINT('Ctrl Pts',(-0.0881142830049797,0.102747609761224,
1.28551003991283));
#14469=CARTESIAN_POINT('Ctrl Pts',(-0.117534109666069,0.0315207854174475,
1.29029707038035));
#14470=CARTESIAN_POINT('Ctrl Pts',(-0.117823716245033,-0.000102811805890825,
1.29243671147362));
#14471=CARTESIAN_POINT('Origin',(0.,0.,-0.0924367114736175));
#14472=CARTESIAN_POINT('',(-0.117957988745754,-3.12301727557783E-5,1.18256328852638));
#14473=CARTESIAN_POINT('',(-0.117793553451004,0.000106755881474893,1.19243671147362));
#14474=CARTESIAN_POINT('',(-0.117775,2.85464118895969E-14,-0.0924367114736175));
#14475=CARTESIAN_POINT('Ctrl Pts',(-0.117957988745754,-3.12301727557569E-5,
1.18256328852638));
#14476=CARTESIAN_POINT('Ctrl Pts',(-0.117964007145535,-0.00173159226684161,
1.18267867767044));
#14477=CARTESIAN_POINT('Ctrl Pts',(-0.117160216762375,-0.0424221720604921,
1.1854403966936));
#14478=CARTESIAN_POINT('Ctrl Pts',(-0.0703321751825429,-0.12013338809653,
1.19084844559586));
#14479=CARTESIAN_POINT('Ctrl Pts',(0.0627954496153871,-0.124239193932754,
1.19878743523316));
#14480=CARTESIAN_POINT('Ctrl Pts',(0.138438143943654,-0.0146125323915816,
1.20672642487047));
#14481=CARTESIAN_POINT('Ctrl Pts',(0.0873502052771435,0.108390901091839,
1.21466541450777));
#14482=CARTESIAN_POINT('Ctrl Pts',(-0.043700859820065,0.132169893139269,
1.22260440414508));
#14483=CARTESIAN_POINT('Ctrl Pts',(-0.112119660921406,0.0591163174148552,
1.22857036215128));
#14484=CARTESIAN_POINT('Ctrl Pts',(-0.117839104743291,0.0100747194789664,
1.23188999027838));
#14485=CARTESIAN_POINT('Ctrl Pts',(-0.11774949833287,0.000107383800510997,
1.23256328852638));
#14486=CARTESIAN_POINT('Ctrl Pts',(-0.117793553451004,0.000106755881474891,
1.19243671147362));
#14487=CARTESIAN_POINT('Ctrl Pts',(-0.117510050331475,-0.0305433296418112,
1.19450912059683));
#14488=CARTESIAN_POINT('Ctrl Pts',(-0.0896091397727994,-0.100804620014092,
1.19922891909429));
#14489=CARTESIAN_POINT('Ctrl Pts',(0.0288222657999454,-0.136209964735594,
1.20659610696603));
#14490=CARTESIAN_POINT('Ctrl Pts',(0.130092623711363,-0.0495962373069701,
1.21453827508881));
#14491=CARTESIAN_POINT('Ctrl Pts',(0.112184773380136,0.082452738709893,
1.22248044321158));
#14492=CARTESIAN_POINT('Ctrl Pts',(-0.00849585454694533,0.138966535376798,
1.23042261133437));
#14493=CARTESIAN_POINT('Ctrl Pts',(-0.103054997843392,0.079672038485689,
1.23707470075504));
#14494=CARTESIAN_POINT('Ctrl Pts',(-0.11756927027536,0.0201573447738481,
1.24107940080146));
#14495=CARTESIAN_POINT('Ctrl Pts',(-0.117581795058195,-8.20683476789562E-6,
1.24243671147361));
#14496=CARTESIAN_POINT('Origin',(0.,0.,-0.0924367114736175));
#14497=CARTESIAN_POINT('',(-0.117657565919426,-8.78585414499747E-5,1.13256328852638));
#14498=CARTESIAN_POINT('',(-0.117937823388479,-5.4172489969917E-5,1.14243671147362));
#14499=CARTESIAN_POINT('',(-0.117775,2.85464118895969E-14,-0.0924367114736175));
#14500=CARTESIAN_POINT('Ctrl Pts',(-0.117657565919426,-8.78585414499974E-5,
1.13256328852638));
#14501=CARTESIAN_POINT('Ctrl Pts',(-0.11775046973706,-0.0134980674796043,
1.13346736506249));
#14502=CARTESIAN_POINT('Ctrl Pts',(-0.109441032251172,-0.0660497484721492,
1.13701777147771));
#14503=CARTESIAN_POINT('Ctrl Pts',(-0.0320511128216771,-0.13546723577438,
1.14321450777202));
#14504=CARTESIAN_POINT('Ctrl Pts',(0.0964380908528195,-0.100390938007982,
1.15115349740933));
#14505=CARTESIAN_POINT('Ctrl Pts',(0.136644831685568,0.0265863832644056,
1.15909248704664));
#14506=CARTESIAN_POINT('Ctrl Pts',(0.0517625939920979,0.129225692742072,
1.16703147668394));
#14507=CARTESIAN_POINT('Ctrl Pts',(-0.0785823129332351,0.113795317289389,
1.17485507717719));
#14508=CARTESIAN_POINT('Ctrl Pts',(-0.117825981412732,0.0372644419932696,
1.18003234779134));
#14509=CARTESIAN_POINT('Ctrl Pts',(-0.117957988745754,-3.12301727557569E-5,
1.18256328852638));
#14510=CARTESIAN_POINT('Ctrl Pts',(-0.117937823388479,-5.41724899699178E-5,
1.14243671147362));
#14511=CARTESIAN_POINT('Ctrl Pts',(-0.117955293269658,-0.0031110520517566,
1.14264406164367));
#14512=CARTESIAN_POINT('Ctrl Pts',(-0.116460933142332,-0.0451799670343263,
1.14549880118799));
#14513=CARTESIAN_POINT('Ctrl Pts',(-0.0660858892268601,-0.122541963197144,
1.15100093010657));
#14514=CARTESIAN_POINT('Ctrl Pts',(0.0671705316110708,-0.121950798202395,
1.15894309822935));
#14515=CARTESIAN_POINT('Ctrl Pts',(0.138891844802359,-0.00964017357273747,
1.16688526635212));
#14516=CARTESIAN_POINT('Ctrl Pts',(0.0833739592533277,0.111501840422208,
1.17482743447491));
#14517=CARTESIAN_POINT('Ctrl Pts',(-0.0485230383040216,0.130496713571114,
1.18276960259768));
#14518=CARTESIAN_POINT('Ctrl Pts',(-0.113150295826959,0.0561813708375219,
1.18863936159726));
#14519=CARTESIAN_POINT('Ctrl Pts',(-0.117872210070015,0.00861047923971886,
1.19186173122257));
#14520=CARTESIAN_POINT('Ctrl Pts',(-0.117793553451004,0.000106755881474891,
1.19243671147362));
#14521=CARTESIAN_POINT('Origin',(0.,0.,-0.0924367114736175));
#14522=CARTESIAN_POINT('',(-0.117641451221435,8.0229283111194E-5,1.08256328852638));
#14523=CARTESIAN_POINT('',(-0.117630591849015,-7.42484764288953E-5,1.09243671147362));
#14524=CARTESIAN_POINT('',(-0.117775,2.85464118895969E-14,-0.0924367114736175));
#14525=CARTESIAN_POINT('Ctrl Pts',(-0.117641451221435,8.02292831111745E-5,
1.08256328852638));
#14526=CARTESIAN_POINT('Ctrl Pts',(-0.117483998834985,-0.0250372639622414,
1.08425605245455));
#14527=CARTESIAN_POINT('Ctrl Pts',(-0.0972946570053161,-0.0896524615425008,
1.08859514626182));
#14528=CARTESIAN_POINT('Ctrl Pts',(0.00904258428980543,-0.13891320121148,
1.09558056994819));
#14529=CARTESIAN_POINT('Ctrl Pts',(0.121617839487272,-0.067732908692211,
1.1035195595855));
#14530=CARTESIAN_POINT('Ctrl Pts',(0.122860297649024,0.0654522196953821,
1.1114585492228));
#14531=CARTESIAN_POINT('Ctrl Pts',(0.0116325734791967,0.138720326685422,
1.11939753886011));
#14532=CARTESIAN_POINT('Ctrl Pts',(-0.096364912740844,0.0911171059582243,
1.1264324519613));
#14533=CARTESIAN_POINT('Ctrl Pts',(-0.117478530206868,0.0257550656131636,
1.13082103518339));
#14534=CARTESIAN_POINT('Ctrl Pts',(-0.117657565919426,-8.78585414499974E-5,
1.13256328852638));
#14535=CARTESIAN_POINT('Ctrl Pts',(-0.117630591849015,-7.42484764288814E-5,
1.09243671147362));
#14536=CARTESIAN_POINT('Ctrl Pts',(-0.117715241483118,-0.0147626739157663,
1.09342639206478));
#14537=CARTESIAN_POINT('Ctrl Pts',(-0.108350501834675,-0.0686384992808382,
1.0970634620302));
#14538=CARTESIAN_POINT('Ctrl Pts',(-0.0276126195379174,-0.136460326620484,
1.10334792136989));
#14539=CARTESIAN_POINT('Ctrl Pts',(0.0997182217817603,-0.0971604536002107,
1.11129008949267));
#14540=CARTESIAN_POINT('Ctrl Pts',(0.135696927507188,0.0311483765905046,
1.11923225761545));
#14541=CARTESIAN_POINT('Ctrl Pts',(0.0473633069609982,0.130922093830007,
1.12717442573822));
#14542=CARTESIAN_POINT('Ctrl Pts',(-0.0809210029008042,0.111284164335459,
1.13490924369095));
#14543=CARTESIAN_POINT('Ctrl Pts',(-0.117732242679493,0.0359183370635313,
1.13999667226941));
#14544=CARTESIAN_POINT('Ctrl Pts',(-0.117937823388479,-5.41724899699178E-5,
1.14243671147362));
#14545=CARTESIAN_POINT('Origin',(0.,0.,-0.0924367114736175));
#14546=CARTESIAN_POINT('',(-0.117948158721073,4.38502512853227E-5,1.03256328852638));
#14547=CARTESIAN_POINT('',(-0.117667547954054,9.20194976846214E-5,1.04243671147362));
#14548=CARTESIAN_POINT('',(-0.117775,2.85464118895969E-14,-0.0924367114736175));
#14549=CARTESIAN_POINT('Ctrl Pts',(-0.117948158721073,4.38502512853157E-5,
1.03256328852638));
#14550=CARTESIAN_POINT('Ctrl Pts',(-0.117773439871091,-0.0365306738650768,
1.03504473984661));
#14551=CARTESIAN_POINT('Ctrl Pts',(-0.0798690478914953,-0.112422454385097,
1.04017252104593));
#14552=CARTESIAN_POINT('Ctrl Pts',(0.0493427524230464,-0.130168884856471,
1.04794663212436));
#14553=CARTESIAN_POINT('Ctrl Pts',(0.136125055048066,-0.0291310004912345,
1.05588562176166));
#14554=CARTESIAN_POINT('Ctrl Pts',(0.0982941990358779,0.0985743183458784,
1.06382461139897));
#14555=CARTESIAN_POINT('Ctrl Pts',(-0.0295182596522469,0.136041604476578,
1.07176360103627));
#14556=CARTESIAN_POINT('Ctrl Pts',(-0.108818061611988,0.067537217334308,
1.07800982674541));
#14557=CARTESIAN_POINT('Ctrl Pts',(-0.11773014713001,0.0142293884972668,
1.08160972257545));
#14558=CARTESIAN_POINT('Ctrl Pts',(-0.117641451221435,8.02292831111745E-5,
1.08256328852638));
#14559=CARTESIAN_POINT('Ctrl Pts',(-0.117667547954054,9.20194976846197E-5,
1.04243671147362));
#14560=CARTESIAN_POINT('Ctrl Pts',(-0.117475882803567,-0.0261866690710452,
1.04420872248589));
#14561=CARTESIAN_POINT('Ctrl Pts',(-0.0957916308421219,-0.0920126959480487,
1.04862812287242));
#14562=CARTESIAN_POINT('Ctrl Pts',(0.0132451643780021,-0.13859452774087,
1.05569491263321));
#14563=CARTESIAN_POINT('Ctrl Pts',(0.123654649330263,-0.0639797248987874,
1.06363708075599));
#14564=CARTESIAN_POINT('Ctrl Pts',(0.120783771971213,0.0692470788374567,
1.07157924887876));
#14565=CARTESIAN_POINT('Ctrl Pts',(0.00726255089817806,0.139036444335888,
1.07952141700155));
#14566=CARTESIAN_POINT('Ctrl Pts',(-0.0979368667310299,0.0886295245336828,
1.08647390453316));
#14567=CARTESIAN_POINT('Ctrl Pts',(-0.117488804242801,0.0245287720112504,
1.09077900269052));
#14568=CARTESIAN_POINT('Ctrl Pts',(-0.117630591849015,-7.42484764288814E-5,
1.09243671147362));
#14569=CARTESIAN_POINT('Origin',(0.,0.,-0.0924367114736175));
#14570=CARTESIAN_POINT('',(-0.117771476475648,-0.000107683352847938,0.982563288526384));
#14571=CARTESIAN_POINT('',(-0.11796176292438,2.53781033017321E-5,0.992436711473616));
#14572=CARTESIAN_POINT('',(-0.117775,2.85464118895969E-14,-0.0924367114736175));
#14573=CARTESIAN_POINT('Ctrl Pts',(-0.117771476475648,-0.000107683352847945,
0.982563288526384));
#14574=CARTESIAN_POINT('Ctrl Pts',(-0.117856103358663,-0.00933799346614349,
0.983187097359559));
#14575=CARTESIAN_POINT('Ctrl Pts',(-0.112646870919438,-0.057630810124202,
0.986457236071836));
#14576=CARTESIAN_POINT('Ctrl Pts',(-0.0461590140787468,-0.131331607851033,
0.992373704663214));
#14577=CARTESIAN_POINT('Ctrl Pts',(0.0853128637208732,-0.110001641284132,
1.00031269430052));
#14578=CARTESIAN_POINT('Ctrl Pts',(0.138686661656432,0.0120272889735618,
1.00825168393783));
#14579=CARTESIAN_POINT('Ctrl Pts',(0.0651023256631918,0.123046060459907,
1.01619067357513));
#14580=CARTESIAN_POINT('Ctrl Pts',(-0.0680787277209358,0.121424596492465,
1.02412966321244));
#14581=CARTESIAN_POINT('Ctrl Pts',(-0.116790117880403,0.0438975063746073,
1.02958720152952));
#14582=CARTESIAN_POINT('Ctrl Pts',(-0.11795976781127,0.00247402277930658,
1.0323984099675));
#14583=CARTESIAN_POINT('Ctrl Pts',(-0.117948158721073,4.38502512853157E-5,
1.03256328852638));
#14584=CARTESIAN_POINT('Ctrl Pts',(-0.11796176292438,2.53781033017319E-5,
0.992436711473616));
#14585=CARTESIAN_POINT('Ctrl Pts',(-0.117851518882229,-0.0376119105440478,
0.994991052906992));
#14586=CARTESIAN_POINT('Ctrl Pts',(-0.077958511321084,-0.114458475672252,
1.00019278371463));
#14587=CARTESIAN_POINT('Ctrl Pts',(0.0529591494285269,-0.128760265574912,
1.00804190389653));
#14588=CARTESIAN_POINT('Ctrl Pts',(0.136912761112491,-0.0252739657289669,
1.0159840720193));
#14589=CARTESIAN_POINT('Ctrl Pts',(0.0954402180350474,0.101365883217864,
1.02392624014209));
#14590=CARTESIAN_POINT('Ctrl Pts',(-0.0334653697086341,0.135144169424284,
1.03186840826486));
#14591=CARTESIAN_POINT('Ctrl Pts',(-0.109792739119276,0.0652029671457737,
1.03803856537538));
#14592=CARTESIAN_POINT('Ctrl Pts',(-0.117762231070763,0.0130737646421874,
1.04156133311163));
#14593=CARTESIAN_POINT('Ctrl Pts',(-0.117667547954054,9.20194976846197E-5,
1.04243671147362));
#14594=CARTESIAN_POINT('Origin',(0.,0.,-0.0924367114736175));
#14595=CARTESIAN_POINT('',(-0.117585265278523,2.16484251076657E-5,0.932563288526384));
#14596=CARTESIAN_POINT('',(-0.117742563953077,-0.000107211314308964,0.942436711473616));
#14597=CARTESIAN_POINT('',(-0.117775,2.85464118895969E-14,-0.0924367114736175));
#14598=CARTESIAN_POINT('Ctrl Pts',(-0.117585265278523,2.16484251076635E-5,
0.932563288526384));
#14599=CARTESIAN_POINT('Ctrl Pts',(-0.117550805757046,-0.0209622679161363,
0.933975784751614));
#14600=CARTESIAN_POINT('Ctrl Pts',(-0.102172791552808,-0.0813069697478888,
0.938034610855947));
#14601=CARTESIAN_POINT('Ctrl Pts',(-0.00565790085648466,-0.139092177922979,
0.944739766839381));
#14602=CARTESIAN_POINT('Ctrl Pts',(0.113796373024222,-0.0801812402497705,
0.952678756476687));
#14603=CARTESIAN_POINT('Ctrl Pts',(0.129077866376032,0.0521301276928276,
0.960617746113992));
#14604=CARTESIAN_POINT('Ctrl Pts',(0.026197419344502,0.13671993644362,0.968556735751298));
#14605=CARTESIAN_POINT('Ctrl Pts',(-0.0906967139502387,0.0993396518733501,
0.975871916555428));
#14606=CARTESIAN_POINT('Ctrl Pts',(-0.117497098103867,0.02981894716558,
0.980540767480457));
#14607=CARTESIAN_POINT('Ctrl Pts',(-0.117771476475648,-0.000107683352847945,
0.982563288526384));
#14608=CARTESIAN_POINT('Ctrl Pts',(-0.117742563953077,-0.000107211314308957,
0.942436711473616));
#14609=CARTESIAN_POINT('Ctrl Pts',(-0.117833632602859,-0.0103126986533654,
0.943125993953839));
#14610=CARTESIAN_POINT('Ctrl Pts',(-0.111944766202914,-0.0596118697348184,
0.946462665808322));
#14611=CARTESIAN_POINT('Ctrl Pts',(-0.0428565117498991,-0.132465832952297,
0.952446727037066));
#14612=CARTESIAN_POINT('Ctrl Pts',(0.0880997963686447,-0.107806787258123,
0.960388895159846));
#14613=CARTESIAN_POINT('Ctrl Pts',(0.138347640177547,0.0156143509765511,
0.968331063282625));
#14614=CARTESIAN_POINT('Ctrl Pts',(0.061854832590724,0.124731139593481,
0.976273231405407));
#14615=CARTESIAN_POINT('Ctrl Pts',(-0.0713033562375951,0.119581390225944,
0.984215399528185));
#14616=CARTESIAN_POINT('Ctrl Pts',(-0.117322772537986,0.0417718924351975,
0.989603226217589));
#14617=CARTESIAN_POINT('Ctrl Pts',(-0.11796577882491,0.00139640554830399,
0.992343663532733));
#14618=CARTESIAN_POINT('Ctrl Pts',(-0.11796176292438,2.53781033017319E-5,
0.992436711473616));
#14619=CARTESIAN_POINT('Origin',(0.,0.,-0.0924367114736175));
#14620=CARTESIAN_POINT('',(-0.117850913371472,9.6525574830472E-5,0.882563288526384));
#14621=CARTESIAN_POINT('',(-0.117591231449503,3.54948526558943E-5,0.892436711473616));
#14622=CARTESIAN_POINT('',(-0.117775,2.85464118895969E-14,-0.0924367114736175));
#14623=CARTESIAN_POINT('Ctrl Pts',(-0.117850913371472,9.65255748304767E-5,
0.882563288526384));
#14624=CARTESIAN_POINT('Ctrl Pts',(-0.117563006813672,-0.0324172738354332,
0.884764472143669));
#14625=CARTESIAN_POINT('Ctrl Pts',(-0.0867151192651892,-0.104499852648429,
0.889611985640057));
#14626=CARTESIAN_POINT('Ctrl Pts',(0.0353397195745277,-0.134646760160997,
0.897105829015547));
#14627=CARTESIAN_POINT('Ctrl Pts',(0.132293719443212,-0.0433245611326863,
0.905044818652852));
#14628=CARTESIAN_POINT('Ctrl Pts',(0.108141885842356,0.0876583043865096,
0.912983808290157));
#14629=CARTESIAN_POINT('Ctrl Pts',(-0.0150064327997127,0.138395999855801,
0.920922797927463));
#14630=CARTESIAN_POINT('Ctrl Pts',(-0.104951114476159,0.0759553573435841,
0.927449291339539));
#14631=CARTESIAN_POINT('Ctrl Pts',(-0.117615366114572,0.01835136974357,
0.931329454872513));
#14632=CARTESIAN_POINT('Ctrl Pts',(-0.117585265278523,2.16484251076635E-5,
0.932563288526384));
#14633=CARTESIAN_POINT('Ctrl Pts',(-0.117591231449503,3.54948526559117E-5,
0.892436711473616));
#14634=CARTESIAN_POINT('Ctrl Pts',(-0.117532234588281,-0.0218238662162972,
0.893908324374946));
#14635=CARTESIAN_POINT('Ctrl Pts',(-0.101194437785642,-0.0830895288483654,
0.898027326650536));
#14636=CARTESIAN_POINT('Ctrl Pts',(-0.00250162451743248,-0.139203517821528,
0.904793718300386));
#14637=CARTESIAN_POINT('Ctrl Pts',(0.115632500949424,-0.0775435504945224,
0.912735886423165));
#14638=CARTESIAN_POINT('Ctrl Pts',(0.127835376168433,0.0551542754370876,
0.920678054545947));
#14639=CARTESIAN_POINT('Ctrl Pts',(0.0229279137899797,0.137325118854324,
0.928620222668725));
#14640=CARTESIAN_POINT('Ctrl Pts',(-0.0920562790907298,0.0974788594069619,
0.935873108311283));
#14641=CARTESIAN_POINT('Ctrl Pts',(-0.117483857027998,0.0288844367965532,
0.94047860457958));
#14642=CARTESIAN_POINT('Ctrl Pts',(-0.117742563953077,-0.000107211314308957,
0.942436711473616));
#14643=CARTESIAN_POINT('Origin',(0.,0.,-0.0924367114736175));
#14644=CARTESIAN_POINT('',(-0.11789232318732,-8.18790992476613E-5,0.832563288526384));
#14645=CARTESIAN_POINT('',(-0.117872825429845,8.99519344067963E-5,0.842436711473616));
#14646=CARTESIAN_POINT('',(-0.117775,2.85464118895969E-14,-0.0924367114736175));
#14647=CARTESIAN_POINT('Ctrl Pts',(-0.11789232318732,-8.18790992476734E-5,
0.832563288526384));
#14648=CARTESIAN_POINT('Ctrl Pts',(-0.117932494517479,-0.00515170743829337,
0.832906829656623));
#14649=CARTESIAN_POINT('Ctrl Pts',(-0.115332713682068,-0.0492334187378749,
0.835896700665964));
#14650=CARTESIAN_POINT('Ctrl Pts',(-0.059752088941783,-0.125731196083361,
0.841532901554406));
#14651=CARTESIAN_POINT('Ctrl Pts',(0.0732361146625898,-0.118385460722959,
0.849471891191712));
#14652=CARTESIAN_POINT('Ctrl Pts',(0.139181674492094,-0.00266594955618734,
0.857410880829018));
#14653=CARTESIAN_POINT('Ctrl Pts',(0.077715950067195,0.115494055719818,
0.865349870466323));
#14654=CARTESIAN_POINT('Ctrl Pts',(-0.0548934004223171,0.127927168308903,
0.87328886010363));
#14655=CARTESIAN_POINT('Ctrl Pts',(-0.114416768398411,0.0522742940766184,
0.879026666123649));
#14656=CARTESIAN_POINT('Ctrl Pts',(-0.117909136832228,0.0066718045071592,
0.882118142264567));
#14657=CARTESIAN_POINT('Ctrl Pts',(-0.117850913371472,9.65255748304767E-5,
0.882563288526384));
#14658=CARTESIAN_POINT('Ctrl Pts',(-0.117872825429845,8.99519344067998E-5,
0.842436711473616));
#14659=CARTESIAN_POINT('Ctrl Pts',(-0.117591169542271,-0.0331870933343037,
0.844690654796053));
#14660=CARTESIAN_POINT('Ctrl Pts',(-0.0854771005934613,-0.106025606004136,
0.84959198749275));
#14661=CARTESIAN_POINT('Ctrl Pts',(0.0380692928980519,-0.133920149482284,
0.857140709563706));
#14662=CARTESIAN_POINT('Ctrl Pts',(0.133179650076608,-0.0405839661022353,
0.865082877686486));
#14663=CARTESIAN_POINT('Ctrl Pts',(0.106283765719693,0.0899312995767124,
0.873025045809266));
#14664=CARTESIAN_POINT('Ctrl Pts',(-0.0179789669825735,0.138060255849953,
0.880967213932046));
#14665=CARTESIAN_POINT('Ctrl Pts',(-0.105798194743126,0.0742290978659706,
0.887437769153496));
#14666=CARTESIAN_POINT('Ctrl Pts',(-0.117638368248411,0.0175004969839459,
0.891260935000686));
#14667=CARTESIAN_POINT('Ctrl Pts',(-0.117591231449503,3.54948526559117E-5,
0.892436711473616));
#14668=CARTESIAN_POINT('Origin',(0.,0.,-0.0924367114736175));
#14669=CARTESIAN_POINT('',(-0.117598114366551,-4.51832715892789E-5,0.782563288526384));
#14670=CARTESIAN_POINT('',(-0.117874685330111,-8.92836445515327E-5,0.792436711473617));
#14671=CARTESIAN_POINT('',(-0.117775,2.85464118895969E-14,-0.0924367114736175));
#14672=CARTESIAN_POINT('Ctrl Pts',(-0.117598114366551,-4.518327158929E-5,
0.782563288526384));
#14673=CARTESIAN_POINT('Ctrl Pts',(-0.117656123976761,-0.0168608793038394,
0.783695517048678));
#14674=CARTESIAN_POINT('Ctrl Pts',(-0.106420815930739,-0.0729055463807818,
0.787474075450074));
#14675=CARTESIAN_POINT('Ctrl Pts',(-0.0202952816069424,-0.137719814645367,
0.793898963730571));
#14676=CARTESIAN_POINT('Ctrl Pts',(0.104705698854998,-0.0917352845351548,
0.801837953367879));
#14677=CARTESIAN_POINT('Ctrl Pts',(0.133855787965376,0.0382266115373486,
0.809776943005182));
#14678=CARTESIAN_POINT('Ctrl Pts',(0.0404700769297216,0.133194664588195,
0.81771593264249));
#14679=CARTESIAN_POINT('Ctrl Pts',(-0.0843190215395119,0.107398870964955,
0.825311381149555));
#14680=CARTESIAN_POINT('Ctrl Pts',(-0.117623050954756,0.0339016606582783,
0.830260499777521));
#14681=CARTESIAN_POINT('Ctrl Pts',(-0.11789232318732,-8.18790992476734E-5,
0.832563288526384));
#14682=CARTESIAN_POINT('Ctrl Pts',(-0.117874685330111,-8.9283644551537E-5,
0.792436711473617));
#14683=CARTESIAN_POINT('Ctrl Pts',(-0.11792303416021,-0.00583050672374999,
0.7928255958429));
#14684=CARTESIAN_POINT('Ctrl Pts',(-0.114931453360353,-0.0506053896743902,
0.795861869586443));
#14685=CARTESIAN_POINT('Ctrl Pts',(-0.0575513573065257,-0.126774282767806,
0.801545532704245));
#14686=CARTESIAN_POINT('Ctrl Pts',(0.0753527000357912,-0.117071978271622,
0.809487700827026));
#14687=CARTESIAN_POINT('Ctrl Pts',(0.139225942868322,-0.000119714417332432,
0.817429868949805));
#14688=CARTESIAN_POINT('Ctrl Pts',(0.0755539188089132,0.116942220141962,
0.825372037072586));
#14689=CARTESIAN_POINT('Ctrl Pts',(-0.0573332568284509,0.12687306712048,
0.833314205195366));
#14690=CARTESIAN_POINT('Ctrl Pts',(-0.114890414736801,0.0507419104293215,
0.839002429995709));
#14691=CARTESIAN_POINT('Ctrl Pts',(-0.117921990994851,0.00589875908008548,
0.842043265421793));
#14692=CARTESIAN_POINT('Ctrl Pts',(-0.117872825429845,8.99519344067998E-5,
0.842436711473616));
#14693=CARTESIAN_POINT('Origin',(0.,0.,-0.0924367114736175));
#14694=CARTESIAN_POINT('',(-0.11772691567491,0.000105512987197037,0.732563288526384));
#14695=CARTESIAN_POINT('',(-0.117591850253004,-3.65476421498312E-5,0.742436711473616));
#14696=CARTESIAN_POINT('',(-0.117775,2.85464118895969E-14,-0.0924367114736175));
#14697=CARTESIAN_POINT('Ctrl Pts',(-0.11772691567491,0.000105512987197042,
0.732563288526384));
#14698=CARTESIAN_POINT('Ctrl Pts',(-0.117479624464894,-0.0283451130369189,
0.734484204440733));
#14699=CARTESIAN_POINT('Ctrl Pts',(-0.0928318426870313,-0.096374559506161,
0.739051450234184));
#14700=CARTESIAN_POINT('Ctrl Pts',(0.0209425314183671,-0.137622876656644,
0.746265025906738));
#14701=CARTESIAN_POINT('Ctrl Pts',(0.126986869252672,-0.0570349089493802,
0.754204015544043));
#14702=CARTESIAN_POINT('Ctrl Pts',(0.11678343126468,0.0757646090434518,
0.762143005181349));
#14703=CARTESIAN_POINT('Ctrl Pts',(-0.000327234354877375,0.139206819944772,
0.770081994818654));
#14704=CARTESIAN_POINT('Ctrl Pts',(-0.100479183608201,0.0843410365921374,
0.776888755933667));
#14705=CARTESIAN_POINT('Ctrl Pts',(-0.117520539541507,0.0224420334666934,
0.781049187169576));
#14706=CARTESIAN_POINT('Ctrl Pts',(-0.117598114366551,-4.518327158929E-5,
0.782563288526384));
#14707=CARTESIAN_POINT('Ctrl Pts',(-0.117591850253004,-3.65476421498364E-5,
0.742436711473616));
#14708=CARTESIAN_POINT('Ctrl Pts',(-0.117640211257931,-0.0174335619022046,
0.743607926264006));
#14709=CARTESIAN_POINT('Ctrl Pts',(-0.105863856762799,-0.0740921523660566,
0.747426530428656));
#14710=CARTESIAN_POINT('Ctrl Pts',(-0.0182163644075178,-0.138029133036789,
0.753892523967566));
#14711=CARTESIAN_POINT('Ctrl Pts',(0.106128952536144,-0.0901139441634624,
0.761834692090347));
#14712=CARTESIAN_POINT('Ctrl Pts',(0.133249245915149,0.0403548753208232,
0.769776860213125));
#14713=CARTESIAN_POINT('Ctrl Pts',(0.0382995408207276,0.133854483197375,
0.777719028335907));
#14714=CARTESIAN_POINT('Ctrl Pts',(-0.0853693283863186,0.106155717082476,
0.785272312089402));
#14715=CARTESIAN_POINT('Ctrl Pts',(-0.117593892160246,0.0332537408718532,
0.79017820646864));
#14716=CARTESIAN_POINT('Ctrl Pts',(-0.117874685330111,-8.9283644551537E-5,
0.792436711473617));
#14717=CARTESIAN_POINT('Origin',(0.,0.,-0.0924367114736175));
#14718=CARTESIAN_POINT('',(-0.117964947617991,-1.73329198795185E-5,0.682563288526384));
#14719=CARTESIAN_POINT('',(-0.117740574064672,0.000107068518266168,0.692436711473616));
#14720=CARTESIAN_POINT('',(-0.117775,2.85464118895969E-14,-0.0924367114736175));
#14721=CARTESIAN_POINT('Ctrl Pts',(-0.117964947617991,-1.73329198795367E-5,
0.682563288526384));
#14722=CARTESIAN_POINT('Ctrl Pts',(-0.117966864156947,-0.000949576032666658,
0.682626561953687));
#14723=CARTESIAN_POINT('Ctrl Pts',(-0.117534558560489,-0.0408698671952461,
0.685336165260092));
#14724=CARTESIAN_POINT('Ctrl Pts',(-0.0726787294560835,-0.118728463672822,
0.690692098445597));
#14725=CARTESIAN_POINT('Ctrl Pts',(0.0603425395611779,-0.125448888878168,
0.698631088082904));
#14726=CARTESIAN_POINT('Ctrl Pts',(0.138124349154501,-0.0173294538893964,
0.706570077720209));
#14727=CARTESIAN_POINT('Ctrl Pts',(0.0894627833767505,0.106653908470079,
0.714509067357515));
#14728=CARTESIAN_POINT('Ctrl Pts',(-0.0410958292974484,0.133002927094911,
0.72244805699482));
#14729=CARTESIAN_POINT('Ctrl Pts',(-0.111546724107196,0.0606813038481789,
0.728466130717777));
#14730=CARTESIAN_POINT('Ctrl Pts',(-0.117820302634623,0.0108495967181263,
0.731837874561632));
#14731=CARTESIAN_POINT('Ctrl Pts',(-0.11772691567491,0.000105512987197042,
0.732563288526384));
#14732=CARTESIAN_POINT('Ctrl Pts',(-0.117740574064672,0.000107068518266165,
0.692436711473616));
#14733=CARTESIAN_POINT('Ctrl Pts',(-0.117483171888848,-0.0288182833237499,
0.694390256685113));
#14734=CARTESIAN_POINT('Ctrl Pts',(-0.0921515028359353,-0.0973455904149804,
0.698991191270869));
#14735=CARTESIAN_POINT('Ctrl Pts',(0.022691720100341,-0.137364345221032,
0.706239515230886));
#14736=CARTESIAN_POINT('Ctrl Pts',(0.127740337615313,-0.0553740340325759,
0.714181683353665));
#14737=CARTESIAN_POINT('Ctrl Pts',(0.115765682611161,0.077344581120379,
0.722123851476446));
#14738=CARTESIAN_POINT('Ctrl Pts',(-0.00226223072526165,0.139207614056346,
0.730066019599226));
#14739=CARTESIAN_POINT('Ctrl Pts',(-0.101117998472899,0.083225715609228,
0.736836972931616));
#14740=CARTESIAN_POINT('Ctrl Pts',(-0.117530897055598,0.0218902846491045,
0.740960536889746));
#14741=CARTESIAN_POINT('Ctrl Pts',(-0.117591850253004,-3.65476421498364E-5,
0.742436711473616));
#14742=CARTESIAN_POINT('Origin',(0.,0.,-0.0924367114736175));
#14743=CARTESIAN_POINT('',(-0.117676160015555,-9.46906955630148E-5,0.632563288526383));
#14744=CARTESIAN_POINT('',(-0.117962383120995,-2.41598447144192E-5,0.642436711473616));
#14745=CARTESIAN_POINT('',(-0.117775,2.85464118895969E-14,-0.0924367114736175));
#14746=CARTESIAN_POINT('Ctrl Pts',(-0.117676160015555,-9.46906955630045E-5,
0.632563288526383));
#14747=CARTESIAN_POINT('Ctrl Pts',(-0.117771520970562,-0.0127268345011372,
0.633415249345741));
#14748=CARTESIAN_POINT('Ctrl Pts',(-0.110078248258936,-0.064483421762156,
0.636913540044201));
#14749=CARTESIAN_POINT('Ctrl Pts',(-0.0347063025259737,-0.134811417789573,
0.643058160621763));
#14750=CARTESIAN_POINT('Ctrl Pts',(0.0944472082050275,-0.102266175560326,
0.65099715025907));
#14751=CARTESIAN_POINT('Ctrl Pts',(0.137140772714236,0.0238967416356601,
0.658936139896373));
#14752=CARTESIAN_POINT('Ctrl Pts',(0.054291358674537,0.128183829614862,
0.666875129533682));
#14753=CARTESIAN_POINT('Ctrl Pts',(-0.0772016597727435,0.11523146575827,
0.674750845743682));
#14754=CARTESIAN_POINT('Ctrl Pts',(-0.117886707375211,0.0380402955314478,
0.679980232074585));
#14755=CARTESIAN_POINT('Ctrl Pts',(-0.117964947617991,-1.73329198795367E-5,
0.682563288526384));
#14756=CARTESIAN_POINT('Ctrl Pts',(-0.117962383120995,-2.41598447144253E-5,
0.642436711473616));
#14757=CARTESIAN_POINT('Ctrl Pts',(-0.117966033213387,-0.0013279541977536,
0.642525197731959));
#14758=CARTESIAN_POINT('Ctrl Pts',(-0.117355585052125,-0.0416360146359673,
0.645261073364563));
#14759=CARTESIAN_POINT('Ctrl Pts',(-0.0715088964667609,-0.119458592094588,
0.650644338371427));
#14760=CARTESIAN_POINT('Ctrl Pts',(0.0616402393688536,-0.124837327709565,
0.658586506494205));
#14761=CARTESIAN_POINT('Ctrl Pts',(0.138320583400205,-0.0158522461166236,
0.666528674616987));
#14762=CARTESIAN_POINT('Ctrl Pts',(0.0882850628235238,0.107655121482266,
0.674470842739765));
#14763=CARTESIAN_POINT('Ctrl Pts',(-0.0426286451686149,0.132539337972556,
0.682413010862546));
#14764=CARTESIAN_POINT('Ctrl Pts',(-0.111894847147975,0.059748848130285,
0.68840163377383));
#14765=CARTESIAN_POINT('Ctrl Pts',(-0.117831996057943,0.0103805377030848,
0.691742867310853));
#14766=CARTESIAN_POINT('Ctrl Pts',(-0.117740574064672,0.000107068518266165,
0.692436711473616));
#14767=CARTESIAN_POINT('Origin',(0.,0.,-0.0924367114736175));
#14768=CARTESIAN_POINT('',(-0.117626285855324,7.11112359239178E-5,0.582563288526384));
#14769=CARTESIAN_POINT('',(-0.11766919235599,-9.26074537421634E-5,0.592436711473616));
#14770=CARTESIAN_POINT('',(-0.117775,2.85464118895969E-14,-0.0924367114736175));
#14771=CARTESIAN_POINT('Ctrl Pts',(-0.117626285855324,7.11112359239024E-5,
0.582563288526383));
#14772=CARTESIAN_POINT('Ctrl Pts',(-0.117492102008102,-0.0242809575267813,
0.584203936737797));
#14773=CARTESIAN_POINT('Ctrl Pts',(-0.0982512120079041,-0.0881067492982899,
0.588490914828312));
#14774=CARTESIAN_POINT('Ctrl Pts',(0.00631176444456456,-0.139064040754811,
0.595424222797929));
#14775=CARTESIAN_POINT('Ctrl Pts',(0.120263693490807,-0.0701091280034811,
0.603363212435234));
#14776=CARTESIAN_POINT('Ctrl Pts',(0.124122453355413,0.0630258865426945,
0.611302202072541));
#14777=CARTESIAN_POINT('Ctrl Pts',(0.0143556138404206,0.138465021405133,
0.619241191709845));
#14778=CARTESIAN_POINT('Ctrl Pts',(-0.0953630726970595,0.0926558297308384,
0.626328220527794));
#14779=CARTESIAN_POINT('Ctrl Pts',(-0.117475314221613,0.0265106736450616,
0.630768919466639));
#14780=CARTESIAN_POINT('Ctrl Pts',(-0.117676160015555,-9.46906955630045E-5,
0.632563288526383));
#14781=CARTESIAN_POINT('Ctrl Pts',(-0.11766919235599,-9.26074537421669E-5,
0.592436711473616));
#14782=CARTESIAN_POINT('Ctrl Pts',(-0.117764072896019,-0.0130062487266101,
0.593307528153066));
#14783=CARTESIAN_POINT('Ctrl Pts',(-0.109848366281979,-0.0650658641993071,
0.596825734206776));
#14784=CARTESIAN_POINT('Ctrl Pts',(-0.0336977294021144,-0.135086418755761,
0.602991329634746));
#14785=CARTESIAN_POINT('Ctrl Pts',(0.0952657566843092,-0.101529863106778,
0.610933497757526));
#14786=CARTESIAN_POINT('Ctrl Pts',(0.136956022624868,0.025038477707157,
0.618875665880307));
#14787=CARTESIAN_POINT('Ctrl Pts',(0.0531805018142573,0.128669000640787,
0.626817834003085));
#14788=CARTESIAN_POINT('Ctrl Pts',(-0.0778376600742765,0.114584191752874,
0.634671515867523));
#14789=CARTESIAN_POINT('Ctrl Pts',(-0.117856827377429,0.0376798124439797,
0.639877808357699));
#14790=CARTESIAN_POINT('Ctrl Pts',(-0.117962383120995,-2.41598447144253E-5,
0.642436711473616));
#14791=CARTESIAN_POINT('Origin',(0.,0.,-0.0924367114736175));
#14792=CARTESIAN_POINT('',(-0.117934829819181,5.63106208242181E-5,0.532563288526383));
#14793=CARTESIAN_POINT('',(-0.117629301205424,7.34277634442948E-5,0.542436711473615));
#14794=CARTESIAN_POINT('',(-0.117775,2.85464118895969E-14,-0.0924367114736175));
#14795=CARTESIAN_POINT('Ctrl Pts',(-0.117934829819181,5.63106208242166E-5,
0.532563288526383));
#14796=CARTESIAN_POINT('Ctrl Pts',(-0.117723349859012,-0.0357608023914865,
0.534992624129852));
#14797=CARTESIAN_POINT('Ctrl Pts',(-0.0811985738067347,-0.110967619805887,
0.540068289612422));
#14798=CARTESIAN_POINT('Ctrl Pts',(0.0467759446245483,-0.131113145053959,
0.547790284974095));
#14799=CARTESIAN_POINT('Ctrl Pts',(0.135526478334676,-0.031799677225719,
0.555729274611401));
#14800=CARTESIAN_POINT('Ctrl Pts',(0.100211809365564,0.0966242157284558,
0.563668264248707));
#14801=CARTESIAN_POINT('Ctrl Pts',(-0.0268399031138932,0.136595261273209,
0.571607253886012));
#14802=CARTESIAN_POINT('Ctrl Pts',(-0.108142973925314,0.0691035501437442,
0.577905595311905));
#14803=CARTESIAN_POINT('Ctrl Pts',(-0.117708537635025,0.0149983997031143,
0.581557606858695));
#14804=CARTESIAN_POINT('Ctrl Pts',(-0.117626285855324,7.11112359239024E-5,
0.582563288526383));
#14805=CARTESIAN_POINT('Ctrl Pts',(-0.117629301205424,7.34277634442983E-5,
0.542436711473615));
#14806=CARTESIAN_POINT('Ctrl Pts',(-0.11748956090956,-0.0244625652698295,
0.544089858574172));
#14807=CARTESIAN_POINT('Ctrl Pts',(-0.0980201725405651,-0.0884941619373469,
0.548390395048989));
#14808=CARTESIAN_POINT('Ctrl Pts',(0.00702343738442799,-0.139048728244533,
0.555338320898066));
#14809=CARTESIAN_POINT('Ctrl Pts',(0.12066450826877,-0.0694546898587181,
0.563280489020846));
#14810=CARTESIAN_POINT('Ctrl Pts',(0.123764493242992,0.063766979789076,
0.571222657143626));
#14811=CARTESIAN_POINT('Ctrl Pts',(0.0134834875971477,0.13857154491934,
0.579164825266405));
#14812=CARTESIAN_POINT('Ctrl Pts',(-0.0957036897026042,0.092147346049863,
0.586236176709736));
#14813=CARTESIAN_POINT('Ctrl Pts',(-0.117475624432153,0.0262528025703711,
0.590660138778806));
#14814=CARTESIAN_POINT('Ctrl Pts',(-0.11766919235599,-9.26074537421669E-5,
0.592436711473616));
#14815=CARTESIAN_POINT('Origin',(0.,0.,-0.0924367114736175));
#14816=CARTESIAN_POINT('',(-0.117794891956694,-0.000106411733115368,0.482563288526384));
#14817=CARTESIAN_POINT('',(-0.117936566864074,5.52347650140707E-5,0.492436711473616));
#14818=CARTESIAN_POINT('',(-0.117775,2.85464118895969E-14,-0.0924367114736175));
#14819=CARTESIAN_POINT('Ctrl Pts',(-0.117794891956694,-0.000106411733115381,
0.482563288526384));
#14820=CARTESIAN_POINT('Ctrl Pts',(-0.117872998614688,-0.00856127641466401,
0.483134981642805));
#14821=CARTESIAN_POINT('Ctrl Pts',(-0.113184542395844,-0.0560672187853419,
0.486353004638329));
#14822=CARTESIAN_POINT('Ctrl Pts',(-0.0487302328423073,-0.130399425645183,
0.492217357512954));
#14823=CARTESIAN_POINT('Ctrl Pts',(0.0831353173341669,-0.111656458896056,
0.50015634715026));
#14824=CARTESIAN_POINT('Ctrl Pts',(0.13889618212661,0.00930034365552528,
0.508095336787567));
#14825=CARTESIAN_POINT('Ctrl Pts',(0.0675071113591811,0.12174331898465,
0.516034326424871));
#14826=CARTESIAN_POINT('Ctrl Pts',(-0.0656800932930844,0.122738629397884,
0.523973316062178));
#14827=CARTESIAN_POINT('Ctrl Pts',(-0.116384786286051,0.04545243224792,
0.529482970096015));
#14828=CARTESIAN_POINT('Ctrl Pts',(-0.117953719733239,0.00325558390455253,
0.53234629425075));
#14829=CARTESIAN_POINT('Ctrl Pts',(-0.117934829819181,5.63106208242166E-5,
0.532563288526383));
#14830=CARTESIAN_POINT('Ctrl Pts',(-0.117936566864074,5.52347650140663E-5,
0.492436711473616));
#14831=CARTESIAN_POINT('Ctrl Pts',(-0.117728017843002,-0.0358510361847084,
0.494872188995279));
#14832=CARTESIAN_POINT('Ctrl Pts',(-0.0810366231971402,-0.111156550628637,
0.499955055891203));
#14833=CARTESIAN_POINT('Ctrl Pts',(0.0471380885036503,-0.131003351527116,
0.507685312161385));
#14834=CARTESIAN_POINT('Ctrl Pts',(0.135643160584381,-0.031381690295376,
0.515627480284167));
#14835=CARTESIAN_POINT('Ctrl Pts',(0.0998851624184703,0.0969888232104648,
0.523569648406945));
#14836=CARTESIAN_POINT('Ctrl Pts',(-0.0273779061153799,0.136507610615132,
0.531511816529727));
#14837=CARTESIAN_POINT('Ctrl Pts',(-0.108290992649607,0.0687756007668377,
0.537800837551949));
#14838=CARTESIAN_POINT('Ctrl Pts',(-0.117713344367368,0.0148299618267192,
0.541442469199912));
#14839=CARTESIAN_POINT('Ctrl Pts',(-0.117629301205424,7.34277634442983E-5,
0.542436711473615));
#14840=CARTESIAN_POINT('Origin',(0.,0.,-0.0924367114736175));
#14841=CARTESIAN_POINT('',(-0.117582256074849,9.06819982020624E-6,0.432563288526383));
#14842=CARTESIAN_POINT('',(-0.11779560903417,-0.000106574656651148,0.442436711473616));
#14843=CARTESIAN_POINT('',(-0.117775,2.85464118895969E-14,-0.0924367114736175));
#14844=CARTESIAN_POINT('Ctrl Pts',(-0.117582256074849,9.06819982019261E-6,
0.432563288526383));
#14845=CARTESIAN_POINT('Ctrl Pts',(-0.117568373935691,-0.020201912089319,
0.43392366903486));
#14846=CARTESIAN_POINT('Ctrl Pts',(-0.10300922874285,-0.0797477867736473,
0.437930379422439));
#14847=CARTESIAN_POINT('Ctrl Pts',(-0.00838939967687663,-0.138954178686792,
0.44458341968912));
#14848=CARTESIAN_POINT('Ctrl Pts',(0.11219917790857,-0.0824013973067221,
0.452522409326426));
#14849=CARTESIAN_POINT('Ctrl Pts',(0.13007709763057,0.0495842159710775,
0.460461398963732));
#14850=CARTESIAN_POINT('Ctrl Pts',(0.0288783492374893,0.136178877755608,
0.468400388601037));
#14851=CARTESIAN_POINT('Ctrl Pts',(-0.0895654556576369,0.100852400902523,
0.475767685121922));
#14852=CARTESIAN_POINT('Ctrl Pts',(-0.117511448025972,0.0305757367622385,
0.480488651763704));
#14853=CARTESIAN_POINT('Ctrl Pts',(-0.117794891956694,-0.000106411733115381,
0.482563288526384));
#14854=CARTESIAN_POINT('Ctrl Pts',(-0.11779560903417,-0.000106574656651151,
0.442436711473616));
#14855=CARTESIAN_POINT('Ctrl Pts',(-0.117873644338608,-0.00854245500997505,
0.443007130042126));
#14856=CARTESIAN_POINT('Ctrl Pts',(-0.113196618671047,-0.056044542179559,
0.446224937984896));
#14857=CARTESIAN_POINT('Ctrl Pts',(-0.0487473834415776,-0.130413074907061,
0.452090135301926));
#14858=CARTESIAN_POINT('Ctrl Pts',(0.0831820848081396,-0.111645054821459,
0.460032303424706));
#14859=CARTESIAN_POINT('Ctrl Pts',(0.138908217753341,0.00940130521287039,
0.467974471547486));
#14860=CARTESIAN_POINT('Ctrl Pts',(0.0673801526530663,0.121835103839429,
0.475916639670265));
#14861=CARTESIAN_POINT('Ctrl Pts',(-0.0658750545035054,0.12265543075329,
0.483858807793047));
#14862=CARTESIAN_POINT('Ctrl Pts',(-0.116424939330292,0.0453161125527027,
0.489365498394162));
#14863=CARTESIAN_POINT('Ctrl Pts',(-0.11795471279604,0.00317945345687678,
0.492224799621019));
#14864=CARTESIAN_POINT('Ctrl Pts',(-0.117936566864074,5.52347650140663E-5,
0.492436711473616));
#14865=CARTESIAN_POINT('Origin',(0.,0.,-0.0924367114736175));
#14866=CARTESIAN_POINT('',(-0.117828183671793,0.000101754196006455,0.382563288526383));
#14867=CARTESIAN_POINT('',(-0.117581664177921,7.09484545444172E-6,0.392436711473616));
#14868=CARTESIAN_POINT('',(-0.117775,2.85464118895969E-14,-0.0924367114736175));
#14869=CARTESIAN_POINT('Ctrl Pts',(-0.117828183671793,0.000101754196006446,
0.382563288526384));
#14870=CARTESIAN_POINT('Ctrl Pts',(-0.117538790254565,-0.0316580736410773,
0.384712356426916));
#14871=CARTESIAN_POINT('Ctrl Pts',(-0.0879068326507716,-0.103002379129266,
0.38950775420655));
#14872=CARTESIAN_POINT('Ctrl Pts',(0.0326876424682324,-0.135315053971568,
0.396949481865287));
#14873=CARTESIAN_POINT('Ctrl Pts',(0.13141703692502,-0.0459152284901983,
0.404888471502591));
#14874=CARTESIAN_POINT('Ctrl Pts',(0.109843140674695,0.0855168418978295,
0.412827461139898));
#14875=CARTESIAN_POINT('Ctrl Pts',(-0.0122846228212416,0.13866410438033,
0.420766450777203));
#14876=CARTESIAN_POINT('Ctrl Pts',(-0.104166535924894,0.0775181589932739,
0.427345059906032));
#14877=CARTESIAN_POINT('Ctrl Pts',(-0.117595378674006,0.0191142356295008,
0.431277339155758));
#14878=CARTESIAN_POINT('Ctrl Pts',(-0.117582256074849,9.06819982019261E-6,
0.432563288526383));
#14879=CARTESIAN_POINT('Ctrl Pts',(-0.117581664177921,7.09484545444172E-6,
0.392436711473616));
#14880=CARTESIAN_POINT('Ctrl Pts',(-0.117570873504463,-0.0200907396801347,
0.393789460463232));
#14881=CARTESIAN_POINT('Ctrl Pts',(-0.10312708440739,-0.079535468422451,
0.397789598827109));
#14882=CARTESIAN_POINT('Ctrl Pts',(-0.00873482453528946,-0.138951719454826,
0.404437126565246));
#14883=CARTESIAN_POINT('Ctrl Pts',(0.112042812448737,-0.0826455423945668,
0.412379294688026));
#14884=CARTESIAN_POINT('Ctrl Pts',(0.130177722634257,0.049372441998279,
0.420321462810806));
#14885=CARTESIAN_POINT('Ctrl Pts',(0.0290564652212241,0.136160197297018,
0.428263630933586));
#14886=CARTESIAN_POINT('Ctrl Pts',(-0.0895090212855029,0.100936776489487,
0.435635380487856));
#14887=CARTESIAN_POINT('Ctrl Pts',(-0.117511471984497,0.0306096014671689,
0.440359740667866));
#14888=CARTESIAN_POINT('Ctrl Pts',(-0.11779560903417,-0.000106574656651151,
0.442436711473616));
#14889=CARTESIAN_POINT('Origin',(0.,0.,-0.0924367114736175));
#14890=CARTESIAN_POINT('',(-0.117911328466355,-7.22474488887591E-5,0.332563288526384));
#14891=CARTESIAN_POINT('',(-0.117821685414254,0.000103165543095151,0.342436711473616));
#14892=CARTESIAN_POINT('',(-0.117775,2.85464118895969E-14,-0.0924367114736175));
#14893=CARTESIAN_POINT('Ctrl Pts',(-0.117911328466355,-7.22474488887752E-5,
0.332563288526384));
#14894=CARTESIAN_POINT('Ctrl Pts',(-0.117942332027964,-0.00437115939612809,
0.332854713939869));
#14895=CARTESIAN_POINT('Ctrl Pts',(-0.115777752883067,-0.0476754067323583,
0.335792469232457));
#14896=CARTESIAN_POINT('Ctrl Pts',(-0.0622106591311991,-0.12453304658572,
0.341376554404146));
#14897=CARTESIAN_POINT('Ctrl Pts',(0.0708961914151981,-0.119801401679107,
0.349315544041452));
#14898=CARTESIAN_POINT('Ctrl Pts',(0.1391024375543,-0.00539978406154301,
0.357254533678757));
#14899=CARTESIAN_POINT('Ctrl Pts',(0.0799699354250877,0.113944965792994,
0.365193523316063));
#14900=CARTESIAN_POINT('Ctrl Pts',(-0.0523695618881846,0.128980908622551,
0.373132512953369));
#14901=CARTESIAN_POINT('Ctrl Pts',(-0.113921748517257,0.0538356345748906,
0.378922434690143));
#14902=CARTESIAN_POINT('Ctrl Pts',(-0.117895144954496,0.00745050051778832,
0.382066026547814));
#14903=CARTESIAN_POINT('Ctrl Pts',(-0.117828183671793,0.000101754196006446,
0.382563288526384));
#14904=CARTESIAN_POINT('Ctrl Pts',(-0.117821685414254,0.000103165543095145,
0.342436711473616));
#14905=CARTESIAN_POINT('Ctrl Pts',(-0.117532262555972,-0.0314544122979593,
0.344571790884339));
#14906=CARTESIAN_POINT('Ctrl Pts',(-0.0882170202347594,-0.102616110661261,
0.349354259669323));
#14907=CARTESIAN_POINT('Ctrl Pts',(0.0320320385160992,-0.135491055083419,
0.356784117828566));
#14908=CARTESIAN_POINT('Ctrl Pts',(0.131227975626944,-0.0465090949381858,
0.364726285951346));
#14909=CARTESIAN_POINT('Ctrl Pts',(0.110205605501345,0.0850799742312894,
0.372668454074126));
#14910=CARTESIAN_POINT('Ctrl Pts',(-0.0117764211155082,0.138727046407055,
0.380610622196906));
#14911=CARTESIAN_POINT('Ctrl Pts',(-0.10403099481448,0.0777947493501838,
0.387200041330069));
#14912=CARTESIAN_POINT('Ctrl Pts',(-0.117591991327853,0.019241607989002,
0.391142071088973));
#14913=CARTESIAN_POINT('Ctrl Pts',(-0.117581664177921,7.09484545444172E-6,
0.392436711473616));
#14914=CARTESIAN_POINT('Origin',(0.,0.,-0.0924367114736175));
#14915=CARTESIAN_POINT('',(-0.117608153246896,-5.64262068778628E-5,0.282563288526383));
#14916=CARTESIAN_POINT('',(-0.117918861549493,-6.80329776671096E-5,0.292436711473615));
#14917=CARTESIAN_POINT('',(-0.117775,2.85464118895969E-14,-0.0924367114736175));
#14918=CARTESIAN_POINT('Ctrl Pts',(-0.117608153246896,-5.64262068778604E-5,
0.282563288526383));
#14919=CARTESIAN_POINT('Ctrl Pts',(-0.117677606263852,-0.0160946837114709,
0.283643401331924));
#14920=CARTESIAN_POINT('Ctrl Pts',(-0.107144424846824,-0.0713401098021974,
0.287369844016567));
#14921=CARTESIAN_POINT('Ctrl Pts',(-0.0229969941138309,-0.137294515779738,
0.293742616580312));
#14922=CARTESIAN_POINT('Ctrl Pts',(0.102883268653204,-0.0937746172089793,
0.301681606217617));
#14923=CARTESIAN_POINT('Ctrl Pts',(0.134580950019115,0.0355895166223291,
0.309620595854923));
#14924=CARTESIAN_POINT('Ctrl Pts',(0.0430789950773988,0.13237388709478,
0.317559585492229));
#14925=CARTESIAN_POINT('Ctrl Pts',(-0.0830523456774332,0.10887452531409,
0.325207149716049));
#14926=CARTESIAN_POINT('Ctrl Pts',(-0.11766079978112,0.0346657214219864,
0.330208384060767));
#14927=CARTESIAN_POINT('Ctrl Pts',(-0.117911328466355,-7.22474488887752E-5,
0.332563288526384));
#14928=CARTESIAN_POINT('Ctrl Pts',(-0.117918861549493,-6.80329776671157E-5,
0.292436711473616));
#14929=CARTESIAN_POINT('Ctrl Pts',(-0.117946256357307,-0.00405052459867665,
0.292706731931186));
#14930=CARTESIAN_POINT('Ctrl Pts',(-0.11595553950755,-0.0470512577090033,
0.295624141763016));
#14931=CARTESIAN_POINT('Ctrl Pts',(-0.0631725212350128,-0.124068972994571,
0.301188940969106));
#14932=CARTESIAN_POINT('Ctrl Pts',(0.0700327441786229,-0.12032993078169,
0.309131109091886));
#14933=CARTESIAN_POINT('Ctrl Pts',(0.139080821187468,-0.00635631000930847,
0.317073277214666));
#14934=CARTESIAN_POINT('Ctrl Pts',(0.0807165776729536,0.11344034374014,
0.325015445337446));
#14935=CARTESIAN_POINT('Ctrl Pts',(-0.0515923433190751,0.129313988454311,
0.332957613460226));
#14936=CARTESIAN_POINT('Ctrl Pts',(-0.113774867115171,0.0543021652640841,
0.338764702172283));
#14937=CARTESIAN_POINT('Ctrl Pts',(-0.117891132111753,0.00767537174388221,
0.341924401510079));
#14938=CARTESIAN_POINT('Ctrl Pts',(-0.117821685414254,0.000103165543095145,
0.342436711473616));
#14939=CARTESIAN_POINT('Origin',(0.,0.,-0.0924367114736175));
#14940=CARTESIAN_POINT('',(-0.117705188630573,0.000102098618198066,0.232563288526383));
#14941=CARTESIAN_POINT('',(-0.1176142238744,-6.23262858038681E-5,0.242436711473616));
#14942=CARTESIAN_POINT('',(-0.117775,2.85464118895969E-14,-0.0924367114736175));
#14943=CARTESIAN_POINT('Ctrl Pts',(-0.117705188630573,0.000102098618198071,
0.232563288526383));
#14944=CARTESIAN_POINT('Ctrl Pts',(-0.117475649963863,-0.0275896003179174,
0.234432088723979));
#14945=CARTESIAN_POINT('Ctrl Pts',(-0.0938913217252411,-0.0948462909608301,
0.238947218800678));
#14946=CARTESIAN_POINT('Ctrl Pts',(0.0182347644767634,-0.138007750384372,
0.246108678756477));
#14947=CARTESIAN_POINT('Ctrl Pts',(0.125841858853055,-0.0595186723796334,
0.254047668393783));
#14948=CARTESIAN_POINT('Ctrl Pts',(0.118249355954961,0.073455671106145,
0.261986658031089));
#14949=CARTESIAN_POINT('Ctrl Pts',(0.00240767183786234,0.139186381940956,
0.269925647668394));
#14950=CARTESIAN_POINT('Ctrl Pts',(-0.0995777503027144,0.0858938305448248,
0.27678452450016));
#14951=CARTESIAN_POINT('Ctrl Pts',(-0.117507442931816,0.0231998416616275,
0.280997071452822));
#14952=CARTESIAN_POINT('Ctrl Pts',(-0.117608153246896,-5.64262068778604E-5,
0.282563288526383));
#14953=CARTESIAN_POINT('Ctrl Pts',(-0.1176142238744,-6.2326285803882E-5,
0.242436711473616));
#14954=CARTESIAN_POINT('Ctrl Pts',(-0.117689148257971,-0.0156863246439697,
0.243489062352292));
#14955=CARTESIAN_POINT('Ctrl Pts',(-0.107519643382358,-0.0705218816827611,
0.247188802605229));
#14956=CARTESIAN_POINT('Ctrl Pts',(-0.024381182195918,-0.137074561658528,
0.253535932232426));
#14957=CARTESIAN_POINT('Ctrl Pts',(0.101985705091022,-0.094777599970642,
0.261478100355206));
#14958=CARTESIAN_POINT('Ctrl Pts',(0.134923209124943,0.0343453801629359,
0.269420268477986));
#14959=CARTESIAN_POINT('Ctrl Pts',(0.0442571924125319,0.132004463632409,
0.277362436600766));
#14960=CARTESIAN_POINT('Ctrl Pts',(-0.0824920331482911,0.109525057495754,
0.285034584265976));
#14961=CARTESIAN_POINT('Ctrl Pts',(-0.117677666622401,0.0349954280503056,
0.290059342556926));
#14962=CARTESIAN_POINT('Ctrl Pts',(-0.117918861549493,-6.80329776671157E-5,
0.292436711473616));
#14963=CARTESIAN_POINT('Origin',(0.,0.,-0.0924367114736175));
#14964=CARTESIAN_POINT('',(-0.117967994073432,-3.0724305424694E-6,0.182563288526383));
#14965=CARTESIAN_POINT('',(-0.117691121003631,9.91971943564221E-5,0.192436711473615));
#14966=CARTESIAN_POINT('',(-0.117775,2.85464118895969E-14,-0.0924367114736175));
#14967=CARTESIAN_POINT('Ctrl Pts',(-0.117967994073432,-3.07243054247449E-6,
0.182563288526383));
#14968=CARTESIAN_POINT('Ctrl Pts',(-0.117968057042159,-0.000167453844217198,
0.182574446236933));
#14969=CARTESIAN_POINT('Ctrl Pts',(-0.117893299674953,-0.0393189363008842,
0.185231933826584));
#14970=CARTESIAN_POINT('Ctrl Pts',(-0.0749972298318695,-0.11727771015962,
0.190535751295337));
#14971=CARTESIAN_POINT('Ctrl Pts',(0.0578663373665801,-0.126610160769685,
0.198474740932643));
#14972=CARTESIAN_POINT('Ctrl Pts',(0.13775723856723,-0.0200396862227523,
0.206413730569949));
#14973=CARTESIAN_POINT('Ctrl Pts',(0.091540828968026,0.104875747581476,
0.214352720207254));
#14974=CARTESIAN_POINT('Ctrl Pts',(-0.0384749358425138,0.133784622116252,
0.22229170984456));
#14975=CARTESIAN_POINT('Ctrl Pts',(-0.110955338697302,0.0622468391270206,
0.22836189928427));
#14976=CARTESIAN_POINT('Ctrl Pts',(-0.11780069007939,0.0116234575531164,
0.231785758844877));
#14977=CARTESIAN_POINT('Ctrl Pts',(-0.117705188630573,0.000102098618198071,
0.232563288526383));
#14978=CARTESIAN_POINT('Ctrl Pts',(-0.117691121003631,9.91971943564221E-5,
0.192436711473615));
#14979=CARTESIAN_POINT('Ctrl Pts',(-0.117474218986382,-0.0270951350261672,
0.194271392773399));
#14980=CARTESIAN_POINT('Ctrl Pts',(-0.0945676524372527,-0.0938598508209937,
0.198753463447442));
#14981=CARTESIAN_POINT('Ctrl Pts',(0.0165156171993534,-0.138242945169174,
0.205882923495746));
#14982=CARTESIAN_POINT('Ctrl Pts',(0.125131592687617,-0.061040658666823,
0.213825091618526));
#14983=CARTESIAN_POINT('Ctrl Pts',(0.119114174013628,0.0720811421096423,
0.221767259741306));
#14984=CARTESIAN_POINT('Ctrl Pts',(0.0039759348809324,0.139169211541763,
0.229709427864086));
#14985=CARTESIAN_POINT('Ctrl Pts',(-0.0990660356104632,0.0867677816679632,
0.236599245108189));
#14986=CARTESIAN_POINT('Ctrl Pts',(-0.117500661679058,0.0236188235484957,
0.240841672978032));
#14987=CARTESIAN_POINT('Ctrl Pts',(-0.1176142238744,-6.2326285803882E-5,
0.242436711473616));
#14988=CARTESIAN_POINT('Origin',(0.,0.,-0.0924367114736175));
#14989=CARTESIAN_POINT('',(-0.117696212882312,-0.000100181105204699,0.132563288526383));
#14990=CARTESIAN_POINT('',(-0.117967699956222,8.3697257429456E-6,0.142436711473616));
#14991=CARTESIAN_POINT('',(-0.117775,2.85464118895969E-14,-0.0924367114736175));
#14992=CARTESIAN_POINT('Ctrl Pts',(-0.117696212882312,-0.000100181105204706,
0.132563288526383));
#14993=CARTESIAN_POINT('Ctrl Pts',(-0.117792074781153,-0.0119544960022407,
0.133363133628988));
#14994=CARTESIAN_POINT('Ctrl Pts',(-0.110696412003459,-0.0629173266909915,
0.136809308610694));
#14995=CARTESIAN_POINT('Ctrl Pts',(-0.0373480950846616,-0.134103559412242,
0.142901813471503));
#14996=CARTESIAN_POINT('Ctrl Pts',(0.0924198687735613,-0.104101940294199,
0.150840803108809));
#14997=CARTESIAN_POINT('Ctrl Pts',(0.137583777756591,0.0211978768359354,
0.158779792746114));
#14998=CARTESIAN_POINT('Ctrl Pts',(0.0567991668878991,0.127092487218924,
0.16671878238342));
#14999=CARTESIAN_POINT('Ctrl Pts',(-0.0757945745091616,0.116657324056303,
0.174646614310176));
#15000=CARTESIAN_POINT('Ctrl Pts',(-0.117953122434976,0.0388197061692436,
0.179928116357831));
#15001=CARTESIAN_POINT('Ctrl Pts',(-0.117967994073432,-3.07243054247449E-6,
0.182563288526383));
#15002=CARTESIAN_POINT('Ctrl Pts',(-0.117967699956222,8.3697257429579E-6,
0.142436711473616));
#15003=CARTESIAN_POINT('Ctrl Pts',(-0.117928252023989,-0.038547130539091,
0.145053723194506));
#15004=CARTESIAN_POINT('Ctrl Pts',(-0.0762804946418446,-0.116178754198862,
0.150318124289656));
#15005=CARTESIAN_POINT('Ctrl Pts',(0.0559861945572589,-0.127473226882309,
0.158229914759066));
#15006=CARTESIAN_POINT('Ctrl Pts',(0.137471621702818,-0.0220324926503626,
0.166172082881846));
#15007=CARTESIAN_POINT('Ctrl Pts',(0.0930189202108026,0.103592267873211,
0.174114251004626));
#15008=CARTESIAN_POINT('Ctrl Pts',(-0.0366486683060043,0.134315868829211,
0.182056419127406));
#15009=CARTESIAN_POINT('Ctrl Pts',(-0.110544190454925,0.0633195416932908,
0.188163905950403));
#15010=CARTESIAN_POINT('Ctrl Pts',(-0.11778720200735,0.0121454601492482,
0.191624003399139));
#15011=CARTESIAN_POINT('Ctrl Pts',(-0.117691121003631,9.91971943564221E-5,
0.192436711473615));
#15012=CARTESIAN_POINT('Origin',(0.,0.,-0.0924367114736175));
#15013=CARTESIAN_POINT('',(-0.117613109409711,6.11591708146705E-5,0.0825632885263832));
#15014=CARTESIAN_POINT('',(-0.117715749944134,-0.000104199409386274,0.0924367114736155));
#15015=CARTESIAN_POINT('',(-0.117775,2.85464118895969E-14,-0.0924367114736175));
#15016=CARTESIAN_POINT('Ctrl Pts',(-0.117613109409711,6.11591708146765E-5,
0.0825632885263832));
#15017=CARTESIAN_POINT('Ctrl Pts',(-0.117502393620717,-0.0235240259785673,
0.0841518210210431));
#15018=CARTESIAN_POINT('Ctrl Pts',(-0.0991849320095013,-0.0865581493706475,
0.088386683394805));
#15019=CARTESIAN_POINT('Ctrl Pts',(0.00357853460314598,-0.139161043603659,
0.0952678756476685));
#15020=CARTESIAN_POINT('Ctrl Pts',(0.118863112008681,-0.0724583686054966,
0.103206865284975));
#15021=CARTESIAN_POINT('Ctrl Pts',(0.125336705278751,0.0605752693714656,
0.11114585492228));
#15022=CARTESIAN_POINT('Ctrl Pts',(0.0170731091066207,0.138156245709763,
0.119084844559586));
#15023=CARTESIAN_POINT('Ctrl Pts',(-0.094337657277608,0.0941904991302726,
0.126223989094287));
#15024=CARTESIAN_POINT('Ctrl Pts',(-0.11747491061231,0.0272661325996615,
0.130716803749886));
#15025=CARTESIAN_POINT('Ctrl Pts',(-0.117696212882312,-0.000100181105204706,
0.132563288526383));
#15026=CARTESIAN_POINT('Ctrl Pts',(-0.117715749944134,-0.000104199409386274,
0.0924367114736155));
#15027=CARTESIAN_POINT('Ctrl Pts',(-0.117810584636384,-0.011244028442556,
0.0931886642413524));
#15028=CARTESIAN_POINT('Ctrl Pts',(-0.111246641208053,-0.0614941526881817,
0.0965880063833492));
#15029=CARTESIAN_POINT('Ctrl Pts',(-0.0397151780004399,-0.133441281507892,
0.102634737899606));
#15030=CARTESIAN_POINT('Ctrl Pts',(0.0906220264938673,-0.105695447092796,
0.110576906022386));
#15031=CARTESIAN_POINT('Ctrl Pts',(0.137940159127448,0.0188783162799928,
0.118519074145166));
#15032=CARTESIAN_POINT('Ctrl Pts',(0.0588909273047484,0.126157580947307,
0.126461242267946));
#15033=CARTESIAN_POINT('Ctrl Pts',(-0.074108440039672,0.117863552156501,
0.134403410390726));
#15034=CARTESIAN_POINT('Ctrl Pts',(-0.117763087033452,0.0399060678969832,
0.139728566792616));
#15035=CARTESIAN_POINT('Ctrl Pts',(-0.117968157858494,0.000455912857932787,
0.142406333820246));
#15036=CARTESIAN_POINT('Ctrl Pts',(-0.117967699956222,8.3697257429579E-6,
0.142436711473616));
#15037=CARTESIAN_POINT('Origin',(0.,0.,-0.0924367114736175));
#15038=CARTESIAN_POINT('',(-0.117917485785546,7.60014832213593E-5,0.0325632885263832));
#15039=CARTESIAN_POINT('',(-0.117600989619072,5.04992496179954E-5,0.0424367114736154));
#15040=CARTESIAN_POINT('',(-0.117775,2.85464118895969E-14,-0.0924367114736175));
#15041=CARTESIAN_POINT('Ctrl Pts',(-0.117917485785546,7.60014832213644E-5,
0.0325632885263832));
#15042=CARTESIAN_POINT('Ctrl Pts',(-0.117676727567847,-0.0349830640657269,
0.0349405084130983));
#15043=CARTESIAN_POINT('Ctrl Pts',(-0.0825043195215805,-0.109517225708346,
0.0399640581789154));
#15044=CARTESIAN_POINT('Ctrl Pts',(0.0441923146003338,-0.131999388615902,
0.0476339378238343));
#15045=CARTESIAN_POINT('Ctrl Pts',(0.134874939024977,-0.034459980695041,
0.0555729274611401));
#15046=CARTESIAN_POINT('Ctrl Pts',(0.102091080224759,0.094638871230671,
0.0635119170984456));
#15047=CARTESIAN_POINT('Ctrl Pts',(-0.0241513666277066,0.137095110112719,
0.0714509067357516));
#15048=CARTESIAN_POINT('Ctrl Pts',(-0.107448046275642,0.0706698818446754,
0.0778013638783972));
#15049=CARTESIAN_POINT('Ctrl Pts',(-0.117686834607281,0.0157664388843013,
0.0815054911419412));
#15050=CARTESIAN_POINT('Ctrl Pts',(-0.117613109409711,6.11591708146765E-5,
0.0825632885263832));
#15051=CARTESIAN_POINT('Ctrl Pts',(-0.117600989619072,5.04992496179954E-5,
0.0424367114736154));
#15052=CARTESIAN_POINT('Ctrl Pts',(-0.117514779739531,-0.0227353060542692,
0.043970994662459));
#15053=CARTESIAN_POINT('Ctrl Pts',(-0.100129952091853,-0.0849605109884783,
0.0481526672255625));
#15054=CARTESIAN_POINT('Ctrl Pts',(0.000787973702835166,-0.139222729671589,
0.054981729162926));
#15055=CARTESIAN_POINT('Ctrl Pts',(0.117431922513572,-0.0747907597173192,
0.0629238972857061));
#15056=CARTESIAN_POINT('Ctrl Pts',(0.126496838785129,0.0581591461343325,
0.070866065408486));
#15057=CARTESIAN_POINT('Ctrl Pts',(0.0196773008918215,0.137828289815661,
0.0788082335312661));
#15058=CARTESIAN_POINT('Ctrl Pts',(-0.0933482651079043,0.0956446566614129,
0.085998448886309));
#15059=CARTESIAN_POINT('Ctrl Pts',(-0.11747670148927,0.0279758085988667,
0.0905412748670923));
#15060=CARTESIAN_POINT('Ctrl Pts',(-0.117715749944134,-0.000104199409386274,
0.0924367114736155));
#15061=CARTESIAN_POINT('Origin',(0.,0.,1.55));
#15062=CARTESIAN_POINT('',(-0.143211704627722,-5.70397197726547E-6,1.50700023576178));
#15063=CARTESIAN_POINT('Ctrl Pts',(-0.0334019664626774,0.112939183906323,
1.532225));
#15064=CARTESIAN_POINT('Ctrl Pts',(-0.0250606930336426,0.115799676338094,
1.53184761307169));
#15065=CARTESIAN_POINT('Ctrl Pts',(-0.0164287086124659,0.117635554524944,
1.53147359869818));
#15066=CARTESIAN_POINT('Ctrl Pts',(-0.00767226928320402,0.118510614220874,
1.53110056493424));
#15067=CARTESIAN_POINT('Ctrl Pts',(-0.0042150196872779,0.118856108509867,
1.53095328237096));
#15068=CARTESIAN_POINT('Ctrl Pts',(-0.000736351480830917,0.119051293525916,
1.53080607672538));
#15069=CARTESIAN_POINT('Ctrl Pts',(0.00274830211697625,0.119097943881266,
1.53065904037218));
#15070=CARTESIAN_POINT('Ctrl Pts',(0.00972321854123044,0.119191319684798,
1.53036473098213));
#15071=CARTESIAN_POINT('Ctrl Pts',(0.0166907125456733,0.118690968429664,
1.53007241075126));
#15072=CARTESIAN_POINT('Ctrl Pts',(0.0235721318645625,0.11762150546261,
1.52978094357425));
#15073=CARTESIAN_POINT('Ctrl Pts',(0.0273478463565568,0.117034709826966,
1.52962102062912));
#15074=CARTESIAN_POINT('Ctrl Pts',(0.0310977188904398,0.116276259986281,
1.52946135449799));
#15075=CARTESIAN_POINT('Ctrl Pts',(0.0348087249896146,0.115347945392283,
1.52930175751644));
#15076=CARTESIAN_POINT('Ctrl Pts',(0.0378768737129624,0.114580442682688,
1.52916980751093));
#15077=CARTESIAN_POINT('Ctrl Pts',(0.0409182562642153,0.113696477767379,
1.52903790896105));
#15078=CARTESIAN_POINT('Ctrl Pts',(0.0439120268522727,0.112701821307647,
1.52890655030309));
#15079=CARTESIAN_POINT('Ctrl Pts',(0.0504861734289241,0.110517613410832,
1.52861809430882));
#15080=CARTESIAN_POINT('Ctrl Pts',(0.0568477403450367,0.107796947733889,
1.528331525126));
#15081=CARTESIAN_POINT('Ctrl Pts',(0.0629211062797432,0.10455513280498,
1.52804576869741));
#15082=CARTESIAN_POINT('Ctrl Pts',(0.0667529140263229,0.102509807084265,
1.52786547926507));
#15083=CARTESIAN_POINT('Ctrl Pts',(0.0704699809867569,0.100256700264741,
1.52768551335768));
#15084=CARTESIAN_POINT('Ctrl Pts',(0.0740519796445933,0.0977963961590643,
1.52750560123222));
#15085=CARTESIAN_POINT('Ctrl Pts',(0.0761474027326905,0.0963571499395001,
1.52740035495562));
#15086=CARTESIAN_POINT('Ctrl Pts',(0.0781972522873126,0.0948464165467323,
1.52729509152825));
#15087=CARTESIAN_POINT('Ctrl Pts',(0.0801950758490376,0.0932655888959708,
1.52718986717129));
#15088=CARTESIAN_POINT('Ctrl Pts',(0.0872135629190184,0.0877120362002772,
1.52682020700562));
#15089=CARTESIAN_POINT('Ctrl Pts',(0.0935342345834078,0.0813437113039547,
1.52645409167081));
#15090=CARTESIAN_POINT('Ctrl Pts',(0.0991216768718319,0.0743433873765979,
1.52608928877518));
#15091=CARTESIAN_POINT('Ctrl Pts',(0.101857856375295,0.0709153174549959,
1.52591064420861));
#15092=CARTESIAN_POINT('Ctrl Pts',(0.104417791592617,0.0673349702414553,
1.52573231437502));
#15093=CARTESIAN_POINT('Ctrl Pts',(0.106794530290299,0.0636205708890664,
1.52555403711528));
#15094=CARTESIAN_POINT('Ctrl Pts',(0.108394385735532,0.0611202951812291,
1.52543403324399));
#15095=CARTESIAN_POINT('Ctrl Pts',(0.109912312880749,0.0585571637778213,
1.52531395827658));
#15096=CARTESIAN_POINT('Ctrl Pts',(0.111341951189028,0.0559432008961949,
1.5251940432238));
#15097=CARTESIAN_POINT('Ctrl Pts',(0.115894033640165,0.0476201345006791,
1.52481222412716));
#15098=CARTESIAN_POINT('Ctrl Pts',(0.119530893641226,0.0388304356906876,
1.52443409356659));
#15099=CARTESIAN_POINT('Ctrl Pts',(0.122195159250079,0.0297595052710396,
1.52405718851832));
#15100=CARTESIAN_POINT('Ctrl Pts',(0.123464283518865,0.0254385629829291,
1.52387764960816));
#15101=CARTESIAN_POINT('Ctrl Pts',(0.124512110981915,0.0210533134598664,
1.52369838877875));
#15102=CARTESIAN_POINT('Ctrl Pts',(0.12532867129748,0.0166220814218575,
1.52351913980531));
#15103=CARTESIAN_POINT('Ctrl Pts',(0.126067828800149,0.012610891624201,
1.52335688207487));
#15104=CARTESIAN_POINT('Ctrl Pts',(0.12661735951473,0.00855739899605222,
1.52319445303817));
#15105=CARTESIAN_POINT('Ctrl Pts',(0.126966826155483,0.00450415768051923,
1.52303280899981));
#15106=CARTESIAN_POINT('Ctrl Pts',(0.127602972227412,-0.00287409603749457,
1.52273856283131));
#15107=CARTESIAN_POINT('Ctrl Pts',(0.12758177643555,-0.010267620141741,
1.52244625042084));
#15108=CARTESIAN_POINT('Ctrl Pts',(0.126865581413421,-0.0175939782534482,
1.52215473434257));
#15109=CARTESIAN_POINT('Ctrl Pts',(0.126426462283551,-0.0220859726121444,
1.52197599770985));
#15110=CARTESIAN_POINT('Ctrl Pts',(0.12572570473317,-0.0265528301690258,
1.52179756043894));
#15111=CARTESIAN_POINT('Ctrl Pts',(0.124776542651163,-0.0309793260681717,
1.52161916036391));
#15112=CARTESIAN_POINT('Ctrl Pts',(0.124151644840291,-0.0338935887106027,
1.52150170748789));
#15113=CARTESIAN_POINT('Ctrl Pts',(0.123418330834614,-0.0367926408403149,
1.52138417707714));
#15114=CARTESIAN_POINT('Ctrl Pts',(0.122581975874549,-0.0396644408336013,
1.52126680258073));
#15115=CARTESIAN_POINT('Ctrl Pts',(0.120074191833131,-0.0482754427851461,
1.52091485884509));
#15116=CARTESIAN_POINT('Ctrl Pts',(0.116656903439717,-0.0566007293654626,
1.52056600333313));
#15117=CARTESIAN_POINT('Ctrl Pts',(0.112443760417108,-0.0645262187619275,
1.52021830866717));
#15118=CARTESIAN_POINT('Ctrl Pts',(0.109356904590302,-0.0703330102694749,
1.51996356219884));
#15119=CARTESIAN_POINT('Ctrl Pts',(0.105841781173658,-0.0759253337267248,
1.51970943888381));
#15120=CARTESIAN_POINT('Ctrl Pts',(0.101930367117466,-0.0812537151913617,
1.51945518067311));
#15121=CARTESIAN_POINT('Ctrl Pts',(0.100130771446666,-0.0837052409256295,
1.51933819945644));
#15122=CARTESIAN_POINT('Ctrl Pts',(0.0982476276828181,-0.0860996963839449,
1.51922123442864));
#15123=CARTESIAN_POINT('Ctrl Pts',(0.0962924325256194,-0.0884227179472683,
1.51910469697823));
#15124=CARTESIAN_POINT('Ctrl Pts',(0.0906946176521128,-0.0950736369671782,
1.51877104482549));
#15125=CARTESIAN_POINT('Ctrl Pts',(0.0844921899154374,-0.101162815315101,
1.51843983772287));
#15126=CARTESIAN_POINT('Ctrl Pts',(0.0777644521522082,-0.106582693579069,
1.51810941878));
#15127=CARTESIAN_POINT('Ctrl Pts',(0.0731067700043679,-0.110334931124879,
1.5178806663426));
#15128=CARTESIAN_POINT('Ctrl Pts',(0.0681966627772886,-0.113766151308436,
1.51765229166508));
#15129=CARTESIAN_POINT('Ctrl Pts',(0.0630541948599911,-0.116833686038022,
1.5174237449583));
#15130=CARTESIAN_POINT('Ctrl Pts',(0.0607686815400033,-0.118197018118406,
1.51732216988754));
#15131=CARTESIAN_POINT('Ctrl Pts',(0.0584414404741937,-0.119485783651375,
1.51722075040181));
#15132=CARTESIAN_POINT('Ctrl Pts',(0.0560784264268894,-0.12069488199044,
1.51711960151386));
#15133=CARTESIAN_POINT('Ctrl Pts',(0.0475595529450054,-0.125053787850271,
1.51675495087613));
#15134=CARTESIAN_POINT('Ctrl Pts',(0.038563113830939,-0.128389854466075,
1.51639315730301));
#15135=CARTESIAN_POINT('Ctrl Pts',(0.0292711048986314,-0.130741856378471,
1.51603205677802));
#15136=CARTESIAN_POINT('Ctrl Pts',(0.0254547302664753,-0.13170786066222,
1.51588374709674));
#15137=CARTESIAN_POINT('Ctrl Pts',(0.0215881861914954,-0.132507324978224,
1.51573555432397));
#15138=CARTESIAN_POINT('Ctrl Pts',(0.0176832233642019,-0.13314066674995,
1.51558732853105));
#15139=CARTESIAN_POINT('Ctrl Pts',(0.0144414794405867,-0.133666441752394,
1.51546427740745));
#15140=CARTESIAN_POINT('Ctrl Pts',(0.0111713231872828,-0.134077605234841,
1.5153411329761));
#15141=CARTESIAN_POINT('Ctrl Pts',(0.00789687394913892,-0.134372952697723,
1.51521845803943));
#15142=CARTESIAN_POINT('Ctrl Pts',(-0.00208492598009478,-0.135273287095873,
1.51484449692866));
#15143=CARTESIAN_POINT('Ctrl Pts',(-0.0121386692885745,-0.135107999768821,
1.51447364169918));
#15144=CARTESIAN_POINT('Ctrl Pts',(-0.0220717676774029,-0.133899092645375,
1.51410356562093));
#15145=CARTESIAN_POINT('Ctrl Pts',(-0.0271373055616968,-0.133282591671289,
1.51391483957382));
#15146=CARTESIAN_POINT('Ctrl Pts',(-0.0321716696217597,-0.132393849601707,
1.51372631615657));
#15147=CARTESIAN_POINT('Ctrl Pts',(-0.0371491047637803,-0.131230566976147,
1.51353768678866));
#15148=CARTESIAN_POINT('Ctrl Pts',(-0.0401763453142056,-0.130523066780721,
1.51342296375255));
#15149=CARTESIAN_POINT('Ctrl Pts',(-0.0431793745847511,-0.129714439573166,
1.51330831773957));
#15150=CARTESIAN_POINT('Ctrl Pts',(-0.0461427198170546,-0.128807808452418,
1.51319405707679));
#15151=CARTESIAN_POINT('Ctrl Pts',(-0.0557912886485991,-0.125855842991896,
1.51282202756853));
#15152=CARTESIAN_POINT('Ctrl Pts',(-0.0650506639775802,-0.121862017750276,
1.51245293010828));
#15153=CARTESIAN_POINT('Ctrl Pts',(-0.0737251756215706,-0.116823260910032,
1.51208446868514));
#15154=CARTESIAN_POINT('Ctrl Pts',(-0.0774533877539874,-0.114657657224767,
1.51192610791459));
#15155=CARTESIAN_POINT('Ctrl Pts',(-0.0810733781510443,-0.112298364258586,
1.51176786463208));
#15156=CARTESIAN_POINT('Ctrl Pts',(-0.0845783705992567,-0.109758519633299,
1.51160955655689));
#15157=CARTESIAN_POINT('Ctrl Pts',(-0.0871260289206952,-0.107912394030924,
1.51149448786814));
#15158=CARTESIAN_POINT('Ctrl Pts',(-0.0896122610481647,-0.105970921032248,
1.51137940572563));
#15159=CARTESIAN_POINT('Ctrl Pts',(-0.0920243025666997,-0.10394826075131,
1.51126473391974));
#15160=CARTESIAN_POINT('Ctrl Pts',(-0.0995315444015674,-0.0976529296958118,
1.51090782920982));
#15161=CARTESIAN_POINT('Ctrl Pts',(-0.106349817996106,-0.090554906599088,
1.51055366538392));
#15162=CARTESIAN_POINT('Ctrl Pts',(-0.112409916721278,-0.0828189535999138,
1.51020021897155));
#15163=CARTESIAN_POINT('Ctrl Pts',(-0.11567060314877,-0.0786565598680515,
1.51001004419521));
#15164=CARTESIAN_POINT('Ctrl Pts',(-0.118711357121208,-0.0743087544864998,
1.50982007711492));
#15165=CARTESIAN_POINT('Ctrl Pts',(-0.121517490738653,-0.0697974244982526,
1.50963000253165));
#15166=CARTESIAN_POINT('Ctrl Pts',(-0.123184827969132,-0.0671169005197731,
1.50951706477726));
#15167=CARTESIAN_POINT('Ctrl Pts',(-0.124768226583796,-0.064379797453554,
1.50940414472167));
#15168=CARTESIAN_POINT('Ctrl Pts',(-0.12625918933752,-0.0616017405091787,
1.50929161182319));
#15169=CARTESIAN_POINT('Ctrl Pts',(-0.131254477666307,-0.0522942005345653,
1.50891458411209));
#15170=CARTESIAN_POINT('Ctrl Pts',(-0.135235816373665,-0.0424980109473837,
1.50854057440173));
#15171=CARTESIAN_POINT('Ctrl Pts',(-0.138100316247284,-0.0323932585971084,
1.50816719719795));
#15172=CARTESIAN_POINT('Ctrl Pts',(-0.139428601593765,-0.027707625827389,
1.5079940600046));
#15173=CARTESIAN_POINT('Ctrl Pts',(-0.140516076092011,-0.0229552175461711,
1.50782105881478));
#15174=CARTESIAN_POINT('Ctrl Pts',(-0.14134846970832,-0.01815262603916,
1.50764795577689));
#15175=CARTESIAN_POINT('Ctrl Pts',(-0.141840021659925,-0.0153165600461233,
1.5075457335416));
#15176=CARTESIAN_POINT('Ctrl Pts',(-0.142241997144177,-0.0124651428186592,
1.50744355431084));
#15177=CARTESIAN_POINT('Ctrl Pts',(-0.142550993842162,-0.00961078035088443,
1.50734168592779));
#15178=CARTESIAN_POINT('Ctrl Pts',(-0.142847161918882,-0.00687492249914849,
1.50724404681617));
#15179=CARTESIAN_POINT('Ctrl Pts',(-0.143058332724879,-0.00413406598225375,
1.5071466105924));
#15180=CARTESIAN_POINT('Ctrl Pts',(-0.143182669649515,-0.00139134585336764,
1.50704933585643));
#15181=CARTESIAN_POINT('Ctrl Pts',(-0.143203595382121,-0.00092974984559876,
1.50703296465278));
#15182=CARTESIAN_POINT('Ctrl Pts',(-0.143222061023464,-0.000468100854706259,
1.50701659802318));
#15183=CARTESIAN_POINT('Ctrl Pts',(-0.143238079070951,-6.41379011939899E-6,
1.50700023577028));
#15184=CARTESIAN_POINT('',(-0.00156744678985144,0.146109855568756,1.50365));
#15185=CARTESIAN_POINT('Ctrl Pts',(-0.00156962371672063,0.146072546381438,
1.50365));
#15186=CARTESIAN_POINT('Ctrl Pts',(-0.011711474284147,0.144648739717271,
1.50495065132295));
#15187=CARTESIAN_POINT('Ctrl Pts',(-0.0216501921041044,0.142222471223284,
1.50626105010813));
#15188=CARTESIAN_POINT('Ctrl Pts',(-0.0312062965385204,0.138804788898175,
1.50759029209282));
#15189=CARTESIAN_POINT('Ctrl Pts',(-0.0379863325344082,0.136379950477271,
1.50853338648503));
#15190=CARTESIAN_POINT('Ctrl Pts',(-0.0445735484268955,0.133455002060128,
1.5094859663039));
#15191=CARTESIAN_POINT('Ctrl Pts',(-0.0508923708069948,0.130021662144985,
1.51045128011208));
#15192=CARTESIAN_POINT('Ctrl Pts',(-0.053607485163773,0.128546401418451,
1.51086606268101));
#15193=CARTESIAN_POINT('Ctrl Pts',(-0.0562647183424556,0.126981576978965,
1.51128195276517));
#15194=CARTESIAN_POINT('Ctrl Pts',(-0.0588579379029418,0.125328026221608,
1.51169910067666));
#15195=CARTESIAN_POINT('Ctrl Pts',(-0.0624505046767585,0.123037247762191,
1.51227700458785));
#15196=CARTESIAN_POINT('Ctrl Pts',(-0.0659209207101175,0.120575889029892,
1.51285741907924));
#15197=CARTESIAN_POINT('Ctrl Pts',(-0.0692542752175272,0.117943487410649,
1.51344114883776));
#15198=CARTESIAN_POINT('Ctrl Pts',(-0.0735613784355843,0.114542101371374,
1.51419539934302));
#15199=CARTESIAN_POINT('Ctrl Pts',(-0.0776398170223455,0.110855132244726,
1.51495518495604));
#15200=CARTESIAN_POINT('Ctrl Pts',(-0.0814741368103916,0.106911749311875,
1.51572224163114));
#15201=CARTESIAN_POINT('Ctrl Pts',(-0.0845038784997064,0.103795829845314,
1.51632834224744));
#15202=CARTESIAN_POINT('Ctrl Pts',(-0.087381117690253,0.10051973853988,
1.51693898261853));
#15203=CARTESIAN_POINT('Ctrl Pts',(-0.0900959757046659,0.0970973798321736,
1.51755501917095));
#15204=CARTESIAN_POINT('Ctrl Pts',(-0.0920052356275281,0.0946905606587243,
1.51798825505079));
#15205=CARTESIAN_POINT('Ctrl Pts',(-0.093830595110286,0.092215607777745,
1.51842338946406));
#15206=CARTESIAN_POINT('Ctrl Pts',(-0.0955653742165971,0.0896840982544811,
1.51885969689116));
#15207=CARTESIAN_POINT('Ctrl Pts',(-0.0997851775729162,0.0835262696618028,
1.51992100293214));
#15208=CARTESIAN_POINT('Ctrl Pts',(-0.103479134251024,0.0770231540939269,
1.52099120961793));
#15209=CARTESIAN_POINT('Ctrl Pts',(-0.106606394578922,0.0702509006766953,
1.52207541818308));
#15210=CARTESIAN_POINT('Ctrl Pts',(-0.108879606303698,0.0653281362576702,
1.52286353153598));
#15211=CARTESIAN_POINT('Ctrl Pts',(-0.110852991156964,0.0602629640702717,
1.52365904329275));
#15212=CARTESIAN_POINT('Ctrl Pts',(-0.112503888351057,0.0550849881514033,
1.524463912762));
#15213=CARTESIAN_POINT('Ctrl Pts',(-0.113450017754745,0.0521174894567802,
1.52492518356294));
#15214=CARTESIAN_POINT('Ctrl Pts',(-0.114289979676541,0.0491121240008169,
1.52538965304266));
#15215=CARTESIAN_POINT('Ctrl Pts',(-0.115015874151616,0.0460903162170444,
1.52585530945224));
#15216=CARTESIAN_POINT('Ctrl Pts',(-0.117053612444637,0.0376074669234184,
1.52716250482259));
#15217=CARTESIAN_POINT('Ctrl Pts',(-0.118206139871793,0.0289652499882669,
1.52848357355921));
#15218=CARTESIAN_POINT('Ctrl Pts',(-0.11838625730212,0.0202925750432425,
1.52982832573377));
#15219=CARTESIAN_POINT('Ctrl Pts',(-0.118492077855379,0.015197303257165,
1.53061837930521));
#15220=CARTESIAN_POINT('Ctrl Pts',(-0.118261361656021,0.0100916471271278,
1.53141660760476));
#15221=CARTESIAN_POINT('Ctrl Pts',(-0.11766859746431,0.00500517689818842,
1.532225));
#15222=CARTESIAN_POINT('',(-0.115079981391543,0.0902137050004572,1.50365));
#15223=CARTESIAN_POINT('Origin',(0.,0.,1.50365));
#15224=CARTESIAN_POINT('Ctrl Pts',(-0.143238079070951,-6.41379011939899E-6,
1.50700023577028));
#15225=CARTESIAN_POINT('Ctrl Pts',(-0.143514357617001,0.00795674345750163,
1.50671802038504));
#15226=CARTESIAN_POINT('Ctrl Pts',(-0.14306421847979,0.0159310909218757,
1.50643710681857));
#15227=CARTESIAN_POINT('Ctrl Pts',(-0.141940608246003,0.023841490005315,
1.50615648267927));
#15228=CARTESIAN_POINT('Ctrl Pts',(-0.141317731836386,0.0282266413964,1.50600091791928));
#15229=CARTESIAN_POINT('Ctrl Pts',(-0.14048752132733,0.0325921818867556,
1.50584544210227));
#15230=CARTESIAN_POINT('Ctrl Pts',(-0.139456452513291,0.0369250818702156,
1.5056898827608));
#15231=CARTESIAN_POINT('Ctrl Pts',(-0.138790989895207,0.0397215809279161,
1.50558948313156));
#15232=CARTESIAN_POINT('Ctrl Pts',(-0.138042009924554,0.0425029011667524,
1.50548910366784));
#15233=CARTESIAN_POINT('Ctrl Pts',(-0.137214434473447,0.0452564915355094,
1.50538902890071));
#15234=CARTESIAN_POINT('Ctrl Pts',(-0.134176751889031,0.0553637675507716,
1.50502169637912));
#15235=CARTESIAN_POINT('Ctrl Pts',(-0.130076454936343,0.0651325632434767,
1.50465723703036));
#15236=CARTESIAN_POINT('Ctrl Pts',(-0.125018127980614,0.0743940890034878,
1.50429344851366));
#15237=CARTESIAN_POINT('Ctrl Pts',(-0.122034683484208,0.0798566160996726,
1.50407888293545));
#15238=CARTESIAN_POINT('Ctrl Pts',(-0.118716925567465,0.0851425936725427,
1.50386455072235));
#15239=CARTESIAN_POINT('Ctrl Pts',(-0.115078604842436,0.0902138214954005,
1.50365));
#15240=CARTESIAN_POINT('',(-0.05,-6.12323399573677E-18,1.6));
#15241=CARTESIAN_POINT('',(-0.1,-1.22464679914735E-17,1.55));
#15242=CARTESIAN_POINT('Origin',(0.,0.,1.6));
#15243=CARTESIAN_POINT('Ctrl Pts',(0.0850780204044575,-0.11908002747757,
-0.0164977839420936));
#15244=CARTESIAN_POINT('Ctrl Pts',(0.124677800165771,-0.0907875342533835,
-0.0138514540629917));
#15245=CARTESIAN_POINT('Ctrl Pts',(0.172751483861701,0.00791416360185712,
-0.00855879430478784));
#15246=CARTESIAN_POINT('Ctrl Pts',(0.0868617128612901,0.149726167188418,
-0.000619804667482127));
#15247=CARTESIAN_POINT('Ctrl Pts',(-0.078614020905812,0.154028602276276,
0.00731918496982359));
#15248=CARTESIAN_POINT('Ctrl Pts',(-0.172087192378165,0.0175525219725009,
0.0152581746071293));
#15249=CARTESIAN_POINT('Ctrl Pts',(-0.108045720411827,-0.135108484733225,
0.0231971642444351));
#15250=CARTESIAN_POINT('Ctrl Pts',(0.0549144151285058,-0.164025561655164,
0.0311361538817407));
#15251=CARTESIAN_POINT('Ctrl Pts',(0.167598788591005,-0.0428207868793744,
0.0390751435190465));
#15252=CARTESIAN_POINT('Ctrl Pts',(0.126860790413016,0.117600499296196,
0.0470141331563521));
#15253=CARTESIAN_POINT('Ctrl Pts',(-0.0300110592737492,0.170357625684536,
0.054953122793658));
#15254=CARTESIAN_POINT('Ctrl Pts',(-0.159409054995301,0.0671687418111174,
0.0628921124309635));
#15255=CARTESIAN_POINT('Ctrl Pts',(-0.142879399887002,-0.0975110083167992,
0.0708311020682695));
#15256=CARTESIAN_POINT('Ctrl Pts',(0.00444677171871267,-0.172924803493063,
0.078770091705575));
#15257=CARTESIAN_POINT('Ctrl Pts',(0.147702113712341,-0.0900384822365835,
0.0867090813428809));
#15258=CARTESIAN_POINT('Ctrl Pts',(0.155746353789385,0.0752722621313087,
0.0946480709801864));
#15259=CARTESIAN_POINT('Ctrl Pts',(0.021215449100004,0.17167621786987,0.102587060617492));
#15260=CARTESIAN_POINT('Ctrl Pts',(-0.132736728465598,0.110922462699857,
0.110526050254798));
#15261=CARTESIAN_POINT('Ctrl Pts',(-0.165177537004225,-0.0513732581591355,
0.118465039892104));
#15262=CARTESIAN_POINT('Ctrl Pts',(-0.0464096261145344,-0.166640254043574,
0.126404029529409));
#15263=CARTESIAN_POINT('Ctrl Pts',(0.114843114370719,-0.129359532685675,
0.134343019166715));
#15264=CARTESIAN_POINT('Ctrl Pts',(0.170964855654229,0.0263409830179588,
0.142282008804021));
#15265=CARTESIAN_POINT('Ctrl Pts',(0.0705799878925336,0.157928129946847,
0.150220998441327));
#15266=CARTESIAN_POINT('Ctrl Pts',(-0.0944160212638482,0.144942899583874,
0.158159988078632));
#15267=CARTESIAN_POINT('Ctrl Pts',(-0.172980633894512,-0.000727622896455919,
0.166098977715938));
#15268=CARTESIAN_POINT('Ctrl Pts',(-0.0931933312323777,-0.145732055885043,
0.174037967353244));
#15269=CARTESIAN_POINT('Ctrl Pts',(0.0719060791645076,-0.157328779695546,
0.181976956990549));
#15270=CARTESIAN_POINT('Ctrl Pts',(0.171180402159323,-0.0249017879745179,
0.189915946627855));
#15271=CARTESIAN_POINT('Ctrl Pts',(0.113750798721884,0.13032108391891,0.197854936265161));
#15272=CARTESIAN_POINT('Ctrl Pts',(-0.0478098650864174,0.16624393501773,
0.205793925902467));
#15273=CARTESIAN_POINT('Ctrl Pts',(-0.16560387403618,0.0499818570245514,
0.213732915539772));
#15274=CARTESIAN_POINT('Ctrl Pts',(-0.131798885878402,-0.112035185581475,
0.221671905177078));
#15275=CARTESIAN_POINT('Ctrl Pts',(0.0226589495323734,-0.171491694067101,
0.229610894814384));
#15276=CARTESIAN_POINT('Ctrl Pts',(0.156374069566079,-0.073959309724122,
0.237549884451689));
#15277=CARTESIAN_POINT('Ctrl Pts',(0.146939445926624,0.0912777539068999,
0.245488874088995));
#15278=CARTESIAN_POINT('Ctrl Pts',(0.00299182995941577,0.172956289510158,
0.253427863726301));
#15279=CARTESIAN_POINT('Ctrl Pts',(-0.143694601292225,0.0963051955349955,
0.261366853363607));
#15280=CARTESIAN_POINT('Ctrl Pts',(-0.15883847309497,-0.0685067047260848,
0.269305843000912));
#15281=CARTESIAN_POINT('Ctrl Pts',(-0.0285766086907934,-0.170605411881679,
0.277244832638218));
#15282=CARTESIAN_POINT('Ctrl Pts',(0.12784518248692,-0.116526556812001,
0.285183822275524));
#15283=CARTESIAN_POINT('Ctrl Pts',(0.167233470900423,0.0442243749325307,
0.293122811912829));
#15284=CARTESIAN_POINT('Ctrl Pts',(0.0535309779628647,0.164490922320707,
0.301061801550136));
#15285=CARTESIAN_POINT('Ctrl Pts',(-0.109175456582181,0.134177303623408,
0.309000791187441));
#15286=CARTESIAN_POINT('Ctrl Pts',(-0.171939242908932,-0.0189664407699395,
0.316939780824747));
#15287=CARTESIAN_POINT('Ctrl Pts',(-0.0773044361184472,-0.154747708493488,
0.324878770462053));
#15288=CARTESIAN_POINT('Ctrl Pts',(0.0880972839194656,-0.148868054644337,
0.332817760099358));
#15289=CARTESIAN_POINT('Ctrl Pts',(0.172851978230285,-0.00670989936239309,
0.340756749736664));
#15290=CARTESIAN_POINT('Ctrl Pts',(0.0993725327910066,0.141590708926387,
0.34869573937397));
#15291=CARTESIAN_POINT('Ctrl Pts',(-0.0650756559739905,0.160274727038081,
0.356634729011275));
#15292=CARTESIAN_POINT('Ctrl Pts',(-0.169951541620772,0.0322382168908211,
0.364573718648582));
#15293=CARTESIAN_POINT('Ctrl Pts',(-0.119248438453561,-0.125310171390688,
0.372512708285886));
#15294=CARTESIAN_POINT('Ctrl Pts',(0.0406184374886585,-0.168145685830938,
0.380451697923193));
#15295=CARTESIAN_POINT('Ctrl Pts',(0.163301917673335,-0.0570553486694088,
0.388390687560498));
#15296=CARTESIAN_POINT('Ctrl Pts',(0.136493684039406,0.106265249940549,
0.396329677197804));
#15297=CARTESIAN_POINT('Ctrl Pts',(-0.0152651628095069,0.172307295063139,
0.404268666835109));
#15298=CARTESIAN_POINT('Ctrl Pts',(-0.153049799296248,0.0806138205455782,
0.412207656472416));
#15299=CARTESIAN_POINT('Ctrl Pts',(-0.150727833715048,-0.0848760818555219,
0.420146646109721));
#15300=CARTESIAN_POINT('Ctrl Pts',(-0.0104248664208018,-0.172667748255674,
0.428085635747027));
#15301=CARTESIAN_POINT('Ctrl Pts',(0.139421351618932,-0.10239392482138,
0.436024625384332));
#15302=CARTESIAN_POINT('Ctrl Pts',(0.16163687742079,0.0616145192729195,
0.443963615021638));
#15303=CARTESIAN_POINT('Ctrl Pts',(0.0358849196425865,0.169219093691645,
0.451902604658944));
#15304=CARTESIAN_POINT('Ctrl Pts',(-0.122717222714247,0.121915185177559,
0.45984159429625));
#15305=CARTESIAN_POINT('Ctrl Pts',(-0.168980158036723,-0.0369937199732681,
0.467780583933555));
#15306=CARTESIAN_POINT('Ctrl Pts',(-0.0605533396431397,-0.162037409833775,
0.475719573570861));
#15307=CARTESIAN_POINT('Ctrl Pts',(0.103305911202344,-0.138746956140414,
0.483658563208167));
#15308=CARTESIAN_POINT('Ctrl Pts',(0.172595680358559,0.0115568269495825,
0.491597552845473));
#15309=CARTESIAN_POINT('Ctrl Pts',(0.0838859329010004,0.151281127008313,
0.499536542482778));
#15310=CARTESIAN_POINT('Ctrl Pts',(-0.0816156370489812,0.152517923263679,
0.507475532120084));
#15311=CARTESIAN_POINT('Ctrl Pts',(-0.172403684765527,0.0141350135070757,
0.51541452175739));
#15312=CARTESIAN_POINT('Ctrl Pts',(-0.105367974675403,-0.137187532379513,
0.523353511394695));
#15313=CARTESIAN_POINT('Ctrl Pts',(0.0581248948911363,-0.162924294448283,
0.531292501032001));
#15314=CARTESIAN_POINT('Ctrl Pts',(0.168408406744046,-0.039515030880773,
0.539231490669306));
#15315=CARTESIAN_POINT('Ctrl Pts',(0.124525564004667,0.120067535316156,
0.547170480306613));
#15316=CARTESIAN_POINT('Ctrl Pts',(-0.0333518982867267,0.169736501696743,
0.555109469943918));
#15317=CARTESIAN_POINT('Ctrl Pts',(-0.160697983451488,0.0640233335761385,
0.563048459581225));
#15318=CARTESIAN_POINT('Ctrl Pts',(-0.14093607811848,-0.100298808627811,
0.570987449218529));
#15319=CARTESIAN_POINT('Ctrl Pts',(0.00784314775175556,-0.172804265459278,
0.578926438855836));
#15320=CARTESIAN_POINT('Ctrl Pts',(0.149442509381278,-0.0871192603125336,
0.586865428493141));
#15321=CARTESIAN_POINT('Ctrl Pts',(0.154237495636292,0.0783174569774929,
0.594804418130446));
#15322=CARTESIAN_POINT('Ctrl Pts',(0.0178386252221998,0.172059909850489,
0.602743407767753));
#15323=CARTESIAN_POINT('Ctrl Pts',(-0.134890284021987,0.108293307291099,
0.610682397405058));
#15324=CARTESIAN_POINT('Ctrl Pts',(-0.164136382878957,-0.0546083962682395,
0.618621387042364));
#15325=CARTESIAN_POINT('Ctrl Pts',(-0.0431268722112106,-0.167519855601819,
0.62656037667967));
#15326=CARTESIAN_POINT('Ctrl Pts',(0.117362334288317,-0.127078368017432,
0.634499366316975));
#15327=CARTESIAN_POINT('Ctrl Pts',(0.170414367112955,0.0296946562375699,
0.642438355954282));
#15328=CARTESIAN_POINT('Ctrl Pts',(0.0674637261050104,0.159284257814778,
0.650377345591586));
#15329=CARTESIAN_POINT('Ctrl Pts',(-0.0972453325609638,0.143060037825677,
0.658316335228894));
#15330=CARTESIAN_POINT('Ctrl Pts',(-0.172932953925271,-0.00412584224812367,
0.666255324866198));
#15331=CARTESIAN_POINT('Ctrl Pts',(-0.0903123078403481,-0.147534796506203,
0.674194314503505));
#15332=CARTESIAN_POINT('Ctrl Pts',(0.0749830665657334,-0.155885755782802,
0.68213330414081));
#15333=CARTESIAN_POINT('Ctrl Pts',(0.17163658245605,-0.021533989188811,
0.690072293778116));
#15334=CARTESIAN_POINT('Ctrl Pts',(0.11116857013107,0.132530668686874,0.698011283415421));
#15335=CARTESIAN_POINT('Ctrl Pts',(-0.0510666492692211,0.165272582299639,
0.705950273052727));
#15336=CARTESIAN_POINT('Ctrl Pts',(-0.166553851089581,0.0467187736868841,
0.713889262690032));
#15337=CARTESIAN_POINT('Ctrl Pts',(-0.129572416918314,-0.114602870389546,
0.721828252327339));
#15338=CARTESIAN_POINT('Ctrl Pts',(0.0260236847639906,-0.171013440871999,
0.729767241964644));
#15339=CARTESIAN_POINT('Ctrl Pts',(0.157796886564457,-0.0708729265526718,
0.73770623160195));
#15340=CARTESIAN_POINT('Ctrl Pts',(0.145117853242075,0.0941468947867542,
0.745645221239255));
#15341=CARTESIAN_POINT('Ctrl Pts',(-0.000406629147419015,0.172981686256994,
0.753584210876562));
#15342=CARTESIAN_POINT('Ctrl Pts',(-0.145558870420566,0.0934635991681543,
0.761523200513868));
#15343=CARTESIAN_POINT('Ctrl Pts',(-0.157461941624574,-0.0716140074803496,
0.769462190151172));
#15344=CARTESIAN_POINT('Ctrl Pts',(-0.0252193968429213,-0.17113389830906,
0.777401179788479));
#15345=CARTESIAN_POINT('Ctrl Pts',(0.130109777350283,-0.113992433807847,
0.785340169425784));
#15346=CARTESIAN_POINT('Ctrl Pts',(0.166332367384696,0.0475012914327479,
0.793279159063091));
#15347=CARTESIAN_POINT('Ctrl Pts',(0.0502890745800368,0.165510839842773,
0.801218148700395));
#15348=CARTESIAN_POINT('Ctrl Pts',(-0.111790419467279,0.132006557575396,
0.809157138337702));
#15349=CARTESIAN_POINT('Ctrl Pts',(-0.171533445990104,-0.0223406811520247,
0.817096127975007));
#15350=CARTESIAN_POINT('Ctrl Pts',(-0.0742493586638003,-0.156236557391639,
0.825035117612313));
#15351=CARTESIAN_POINT('Ctrl Pts',(0.0910049278783345,-0.147108572929777,
0.832974107249618));
#15352=CARTESIAN_POINT('Ctrl Pts',(0.172950439922886,-0.00331277195964383,
0.840913096886925));
#15353=CARTESIAN_POINT('Ctrl Pts',(0.0965716772857839,0.143515644700454,
0.848852086524229));
#15354=CARTESIAN_POINT('Ctrl Pts',(-0.0682118374171683,0.158965324406771,
0.856791076161536));
#15355=CARTESIAN_POINT('Ctrl Pts',(-0.170552089827228,0.0288931442238776,
0.864730065798841));
#15356=CARTESIAN_POINT('Ctrl Pts',(-0.116763592698541,-0.127628729319482,
0.872669055436147));
#15357=CARTESIAN_POINT('Ctrl Pts',(0.0439139712140358,-0.167315248138923,
0.880608045073453));
#15358=CARTESIAN_POINT('Ctrl Pts',(0.164391304101163,-0.0538361241500125,
0.888547034710759));
#15359=CARTESIAN_POINT('Ctrl Pts',(0.134379664555536,0.108926281867684,
0.896486024348063));
#15360=CARTESIAN_POINT('Ctrl Pts',(-0.018647348250808,0.17197414204115,
0.904425013985371));
#15361=CARTESIAN_POINT('Ctrl Pts',(-0.154603991719776,0.0775914613336281,
0.912364003622676));
#15362=CARTESIAN_POINT('Ctrl Pts',(-0.149031276472826,-0.0878208845346985,
0.920302993259982));
#15363=CARTESIAN_POINT('Ctrl Pts',(-0.00703064139541984,-0.172839229369798,
0.928241982897287));
#15364=CARTESIAN_POINT('Ctrl Pts',(0.141406064038169,-0.099635105162837,
0.936180972534593));
#15365=CARTESIAN_POINT('Ctrl Pts',(0.160395209035295,0.064778129380991,
0.944119962171899));
#15366=CARTESIAN_POINT('Ctrl Pts',(0.03255353276219,0.169891426011666,0.952058951809204));
#15367=CARTESIAN_POINT('Ctrl Pts',(-0.125088671715395,0.119480765548496,
0.959997941446511));
#15368=CARTESIAN_POINT('Ctrl Pts',(-0.168220770124088,-0.040306347222682,
0.967936931083815));
#15369=CARTESIAN_POINT('Ctrl Pts',(-0.0573582824064844,-0.163195761485875,
0.975875920721122));
#15370=CARTESIAN_POINT('Ctrl Pts',(0.106011781834435,-0.136690640644722,
0.983814910358427));
#15371=CARTESIAN_POINT('Ctrl Pts',(0.17233532526783,0.014945393685262,0.991753899995733));
#15372=CARTESIAN_POINT('Ctrl Pts',(0.0808976893297158,0.152899944371113,
0.999692889633039));
#15373=CARTESIAN_POINT('Ctrl Pts',(-0.0845962369090198,0.150885074902754,
1.00763187927034));
#15374=CARTESIAN_POINT('Ctrl Pts',(-0.172648106016301,0.0107452601904448,
1.01557086890765));
#15375=CARTESIAN_POINT('Ctrl Pts',(-0.102652466413112,-0.13923110380544,
1.02350985854496));
#15376=CARTESIAN_POINT('Ctrl Pts',(0.0613144709582997,-0.161750934398167,
1.03144884818226));
#15377=CARTESIAN_POINT('Ctrl Pts',(0.169152212322519,-0.0361988700648799,
1.03938783781957));
#15378=CARTESIAN_POINT('Ctrl Pts',(0.122142696063681,0.12249077894222,1.04732682745687));
#15379=CARTESIAN_POINT('Ctrl Pts',(-0.0366800874558037,0.169048514669047,
1.05526581709418));
#15380=CARTESIAN_POINT('Ctrl Pts',(-0.161924764760067,0.0608539208677085,
1.06320480673148));
#15381=CARTESIAN_POINT('Ctrl Pts',(-0.138938417355371,-0.103048266896446,
1.07114379636879));
#15382=CARTESIAN_POINT('Ctrl Pts',(0.011236529066559,-0.172616828675865,
1.0790827860061));
#15383=CARTESIAN_POINT('Ctrl Pts',(0.151125203217684,-0.0841665140064042,
1.0870217756434));
#15384=CARTESIAN_POINT('Ctrl Pts',(0.152669111109608,0.0813324759279986,
1.09496076528071));
#15385=CARTESIAN_POINT('Ctrl Pts',(0.0144549108781955,0.172377158228925,
1.10289975491801));
#15386=CARTESIAN_POINT('Ctrl Pts',(-0.136991769602464,0.10562236594946,
1.11083874455532));
#15387=CARTESIAN_POINT('Ctrl Pts',(-0.163031873671196,-0.0578224635832477,
1.11877773419263));
#15388=CARTESIAN_POINT('Ctrl Pts',(-0.0398274706979539,-0.168334790537727,
1.12671672382993));
#15389=CARTESIAN_POINT('Ctrl Pts',(0.119836252144435,-0.124748153491552,
1.13465571346724));
#15390=CARTESIAN_POINT('Ctrl Pts',(0.169798099063322,0.0330368685268242,
1.14259470310454));
#15391=CARTESIAN_POINT('Ctrl Pts',(0.0643214233134591,0.160578901573361,
1.15053369274185));
#15392=CARTESIAN_POINT('Ctrl Pts',(-0.100037107244844,0.141121955420339,
1.15847268237915));
#15393=CARTESIAN_POINT('Ctrl Pts',(-0.172818522111203,-0.00752246920075927,
1.16641167201646));
#15394=CARTESIAN_POINT('Ctrl Pts',(-0.0873964240115842,-0.149280588817046,
1.17435066165376));
#15395=CARTESIAN_POINT('Ctrl Pts',(0.0780311106025284,-0.154382560238235,
1.18228965129107));
#15396=CARTESIAN_POINT('Ctrl Pts',(0.172026511281289,-0.01815787828917,
1.19022864092837));
#15397=CARTESIAN_POINT('Ctrl Pts',(0.10854343062882,0.134689096792963,1.19816763056568));
#15398=CARTESIAN_POINT('Ctrl Pts',(-0.0543037217972188,0.164237434607784,
1.20610662020299));
#15399=CARTESIAN_POINT('Ctrl Pts',(-0.167439538594998,0.0434376569656869,
1.21404560984029));
#15400=CARTESIAN_POINT('Ctrl Pts',(-0.127295933190098,-0.117126318651471,
1.2219845994776));
#15401=CARTESIAN_POINT('Ctrl Pts',(0.0293783748903316,-0.170469176734012,
1.2299235891149));
#15402=CARTESIAN_POINT('Ctrl Pts',(0.159158794190081,-0.0677591865323411,
1.23786257875221));
#15403=CARTESIAN_POINT('Ctrl Pts',(0.143240245273553,0.0969796950995427,
1.24580156838952));
#15404=CARTESIAN_POINT('Ctrl Pts',(-0.00380493129617075,0.172940312320012,
1.25374055802682));
#15405=CARTESIAN_POINT('Ctrl Pts',(-0.147366954032488,0.0905859259858403,
1.26167954766413));
#15406=CARTESIAN_POINT('Ctrl Pts',(-0.156024630070406,-0.074693667330688,
1.26961853730143));
#15407=CARTESIAN_POINT('Ctrl Pts',(-0.0218524503424686,-0.171596327294885,
1.27755752693874));
#15408=CARTESIAN_POINT('Ctrl Pts',(0.132324150022753,-0.111414309889572,
1.28549651657604));
#15409=CARTESIAN_POINT('Ctrl Pts',(0.165367059817933,0.0507598725070622,
1.29343550621335));
#15410=CARTESIAN_POINT('Ctrl Pts',(0.0470277596764783,0.166466870408131,
1.30137449585065));
#15411=CARTESIAN_POINT('Ctrl Pts',(-0.114362231391601,0.129784857201791,
1.30931348548797));
#15412=CARTESIAN_POINT('Ctrl Pts',(-0.171061437441431,-0.0257062980954763,
1.31725247512526));
#15413=CARTESIAN_POINT('Ctrl Pts',(-0.071165620995849,-0.157665099140374,
1.32519146476257));
#15414=CARTESIAN_POINT('Ctrl Pts',(0.0938774439379855,-0.145292307632914,
1.33313045439988));
#15415=CARTESIAN_POINT('Ctrl Pts',(0.172982143233999,8.56343898915854E-5,
1.34106944403719));
#15416=CARTESIAN_POINT('Ctrl Pts',(0.0937335447930804,0.145385183220099,
1.34900843367449));
#15417=CARTESIAN_POINT('Ctrl Pts',(-0.0713216883190155,0.157594562185848,
1.3569474233118));
#15418=CARTESIAN_POINT('Ctrl Pts',(-0.171086806821499,0.0255369173285507,
1.3648864129491));
#15419=CARTESIAN_POINT('Ctrl Pts',(-0.114233673229396,-0.129898019862958,
1.37282540258641));
#15420=CARTESIAN_POINT('Ctrl Pts',(0.0471925482590101,-0.166420232464351,
1.38076439222371));
#15421=CARTESIAN_POINT('Ctrl Pts',(0.165417247017141,-0.0505961085897048,
1.38870338186102));
#15422=CARTESIAN_POINT('Ctrl Pts',(0.132213753266125,0.111545248710567,
1.39664237149832));
#15423=CARTESIAN_POINT('Ctrl Pts',(-0.0220222951247444,0.17157464463752,
1.40458136113563));
#15424=CARTESIAN_POINT('Ctrl Pts',(-0.156098584526576,0.0745390809398717,
1.41252035077293));
#15425=CARTESIAN_POINT('Ctrl Pts',(-0.147277046608992,-0.0907316537045687,
1.42045934041024));
#15426=CARTESIAN_POINT('Ctrl Pts',(-0.00363398118293899,-0.172944250658386,
1.42839833004755));
#15427=CARTESIAN_POINT('Ctrl Pts',(0.143336722904634,-0.0968373407211472,
1.43633731968485));
#15428=CARTESIAN_POINT('Ctrl Pts',(0.159090624036536,0.0679158129692223,
1.44427630932216));
#15429=CARTESIAN_POINT('Ctrl Pts',(0.0292114869387437,0.170499931406899,
1.45221529895946));
#15430=CARTESIAN_POINT('Ctrl Pts',(-0.127415456569397,0.116996902323752,
1.46015428859677));
#15431=CARTESIAN_POINT('Ctrl Pts',(-0.167389576437263,-0.0435971050111283,
1.46809327823408));
#15432=CARTESIAN_POINT('Ctrl Pts',(-0.0541541359620402,-0.164303103757731,
1.47603226787138));
#15433=CARTESIAN_POINT('Ctrl Pts',(0.108701533888403,-0.13455879509903,
1.48397125750869));
#15434=CARTESIAN_POINT('Ctrl Pts',(0.171961157005542,0.0182848320604298,
1.49191024714599));
#15435=CARTESIAN_POINT('Ctrl Pts',(0.0779697431325927,0.154543202561513,
1.4998492367833));
#15436=CARTESIAN_POINT('Ctrl Pts',(-0.0877325682749983,0.149025855561406,
1.5077882264206));
#15437=CARTESIAN_POINT('Ctrl Pts',(-0.144149484752264,0.0548439265155397,
1.51308088617881));
#15438=CARTESIAN_POINT('Ctrl Pts',(-0.146217781693078,0.00621955116994065,
1.51572721605791));
#15439=CARTESIAN_POINT('Ctrl Pts',(0.0795408277542855,-0.111329858282327,
-0.0109985226280624));
#15440=CARTESIAN_POINT('Ctrl Pts',(0.116563307192903,-0.0848787452970238,
-0.00835219274896048));
#15441=CARTESIAN_POINT('Ctrl Pts',(0.16150817751539,0.00739908052493189,
-0.00305953299075667));
#15442=CARTESIAN_POINT('Ctrl Pts',(0.0812084309002137,0.139981433724326,
0.00487945664654907));
#15443=CARTESIAN_POINT('Ctrl Pts',(-0.0734975292821143,0.144003850402812,
0.0128184462838548));
#15444=CARTESIAN_POINT('Ctrl Pts',(-0.160887120581772,0.0164101388376342,
0.0207574359211605));
#15445=CARTESIAN_POINT('Ctrl Pts',(-0.101013704785435,-0.126315124179183,
0.0286964255584662));
#15446=CARTESIAN_POINT('Ctrl Pts',(0.0513403816191153,-0.153350170642076,
0.0366354151957719));
#15447=CARTESIAN_POINT('Ctrl Pts',(0.156690838735662,-0.0400338514845966,
0.0445744048330777));
#15448=CARTESIAN_POINT('Ctrl Pts',(0.118604220350264,0.109946623274354,
0.0525133944703833));
#15449=CARTESIAN_POINT('Ctrl Pts',(-0.0280578283917351,0.15927012049393,
0.0604523841076892));
#15450=CARTESIAN_POINT('Ctrl Pts',(-0.14903412333264,0.0627971513379326,
0.0683913737449947));
#15451=CARTESIAN_POINT('Ctrl Pts',(-0.133580279395553,-0.0911646307683348,
0.0763303633823007));
#15452=CARTESIAN_POINT('Ctrl Pts',(0.0041573593468571,-0.161670216863261,
0.0842693530196062));
#15453=CARTESIAN_POINT('Ctrl Pts',(0.138089113144455,-0.0841784443595545,
0.0922083426569122));
#15454=CARTESIAN_POINT('Ctrl Pts',(0.14560980428584,0.0703732645446943,
0.100147332294218));
#15455=CARTESIAN_POINT('Ctrl Pts',(0.0198346691022095,0.160502893816501,
0.108086321931524));
#15456=CARTESIAN_POINT('Ctrl Pts',(-0.124097730593135,0.103703218031488,
0.116025311568829));
#15457=CARTESIAN_POINT('Ctrl Pts',(-0.154427171169137,-0.0480296962598115,
0.123964301206135));
#15458=CARTESIAN_POINT('Ctrl Pts',(-0.0433891157712434,-0.155794689166463,
0.13190329084344));
#15459=CARTESIAN_POINT('Ctrl Pts',(0.107368699171666,-0.12094033522185,
0.139842280480747));
#15460=CARTESIAN_POINT('Ctrl Pts',(0.15983782968835,0.0246266142906177,
0.147781270118052));
#15461=CARTESIAN_POINT('Ctrl Pts',(0.0659863808909888,0.147649582370873,
0.155720259755358));
#15462=CARTESIAN_POINT('Ctrl Pts',(-0.0882710769349216,0.135509478890084,
0.163659249392663));
#15463=CARTESIAN_POINT('Ctrl Pts',(-0.161722413615419,-0.00068026650363694,
0.171598239029969));
#15464=CARTESIAN_POINT('Ctrl Pts',(-0.0871279640988751,-0.136247273976568,
0.179537228667275));
#15465=CARTESIAN_POINT('Ctrl Pts',(0.0672261652318651,-0.147089240053593,
0.187476218304581));
#15466=CARTESIAN_POINT('Ctrl Pts',(0.160039347628626,-0.023281087390596,
0.195415207941886));
#15467=CARTESIAN_POINT('Ctrl Pts',(0.106347475470598,0.121839305139765,
0.203354197579192));
#15468=CARTESIAN_POINT('Ctrl Pts',(-0.0446982220051161,0.15542416405057,
0.211293187216498));
#15469=CARTESIAN_POINT('Ctrl Pts',(-0.154825760608133,0.0467288526640558,
0.219232176853804));
#15470=CARTESIAN_POINT('Ctrl Pts',(-0.12322092627477,-0.104743520787053,
0.227171166491109));
#15471=CARTESIAN_POINT('Ctrl Pts',(0.0211842211805034,-0.160330379506191,
0.235110156128415));
#15472=CARTESIAN_POINT('Ctrl Pts',(0.146196665995071,-0.0691457639426259,
0.24304914576572));
#15473=CARTESIAN_POINT('Ctrl Pts',(0.137376082602736,0.0853370596399817,
0.250988135403027));
#15474=CARTESIAN_POINT('Ctrl Pts',(0.00279711058556459,0.161699653653757,
0.258927125040332));
#15475=CARTESIAN_POINT('Ctrl Pts',(-0.134342424474264,0.0900372967480426,
0.266866114677638));
#15476=CARTESIAN_POINT('Ctrl Pts',(-0.148500677015507,-0.0640480346713102,
0.274805104314944));
#15477=CARTESIAN_POINT('Ctrl Pts',(-0.0267167371651392,-0.159501779847699,
0.282744093952249));
#15478=CARTESIAN_POINT('Ctrl Pts',(0.119524544542348,-0.108942576944327,
0.290683083589556));
#15479=CARTESIAN_POINT('Ctrl Pts',(0.156349297273321,0.0413460888291301,
0.29862207322686));
#15480=CARTESIAN_POINT('Ctrl Pts',(0.0500469836677093,0.153785243912065,
0.306561062864167));
#15481=CARTESIAN_POINT('Ctrl Pts',(-0.102069913541897,0.125444547784578,
0.314500052501472));
#15482=CARTESIAN_POINT('Ctrl Pts',(-0.160748800211922,-0.0177320345633525,
0.322439042138778));
#15483=CARTESIAN_POINT('Ctrl Pts',(-0.0722731771226978,-0.144676154524232,
0.330378031776084));
#15484=CARTESIAN_POINT('Ctrl Pts',(0.082363586418043,-0.139179170322594,
0.338317021413389));
#15485=CARTESIAN_POINT('Ctrl Pts',(0.16160213133829,-0.00627319426210969,
0.346256011050695));
#15486=CARTESIAN_POINT('Ctrl Pts',(0.0929050003357002,0.132375461215256,
0.354195000688001));
#15487=CARTESIAN_POINT('Ctrl Pts',(-0.0608402912787218,0.149843454232904,
0.362133990325306));
#15488=CARTESIAN_POINT('Ctrl Pts',(-0.158890465884947,0.0301400343429239,
0.370072979962613));
#15489=CARTESIAN_POINT('Ctrl Pts',(-0.1114873084483,-0.117154521356547,
0.378011969599918));
#15490=CARTESIAN_POINT('Ctrl Pts',(0.0379748391485164,-0.157202141877815,
0.385950959237223));
#15491=CARTESIAN_POINT('Ctrl Pts',(0.152673624090564,-0.0533419752763387,
0.39388994887453));
#15492=CARTESIAN_POINT('Ctrl Pts',(0.127610169584502,0.0993491139263089,
0.401828938511835));
#15493=CARTESIAN_POINT('Ctrl Pts',(-0.014271649480085,0.16109289816887,
0.409767928149142));
#15494=CARTESIAN_POINT('Ctrl Pts',(-0.143088751545671,0.0753671745551693,
0.417706917786446));
#15495=CARTESIAN_POINT('Ctrl Pts',(-0.140917908083783,-0.0793520321139836,
0.425645907423752));
#15496=CARTESIAN_POINT('Ctrl Pts',(-0.00974637750615997,-0.161429891732714,
0.433584897061058));
#15497=CARTESIAN_POINT('Ctrl Pts',(0.130347293715478,-0.0957297489831606,
0.441523886698364));
#15498=CARTESIAN_POINT('Ctrl Pts',(0.15111695082405,0.0576044181723055,
0.449462876335669));
#15499=CARTESIAN_POINT('Ctrl Pts',(0.0335493961742207,0.158205688379633,
0.457401865972975));
#15500=CARTESIAN_POINT('Ctrl Pts',(-0.114730331382826,0.113980493419335,
0.465340855610281));
#15501=CARTESIAN_POINT('Ctrl Pts',(-0.157982303542021,-0.03458603167299,
0.473279845247587));
#15502=CARTESIAN_POINT('Ctrl Pts',(-0.0566123040428622,-0.151491415104245,
0.481218834884892));
#15503=CARTESIAN_POINT('Ctrl Pts',(0.0965823799129518,-0.129716790392294,
0.489157824522198));
#15504=CARTESIAN_POINT('Ctrl Pts',(0.161362514281243,0.0108046658515635,
0.497096814159504));
#15505=CARTESIAN_POINT('Ctrl Pts',(0.0784263257203939,0.141435191000425,
0.50503580379681));
#15506=CARTESIAN_POINT('Ctrl Pts',(-0.076303789130349,0.14259149197508,
0.512974793434115));
#15507=CARTESIAN_POINT('Ctrl Pts',(-0.161183014472451,0.0132150544797126,
0.520913783071421));
#15508=CARTESIAN_POINT('Ctrl Pts',(-0.0985102366584373,-0.128258859705,
0.528852772708727));
#15509=CARTESIAN_POINT('Ctrl Pts',(0.0543419114689404,-0.152320577983508,
0.536791762346032));
#15510=CARTESIAN_POINT('Ctrl Pts',(0.157447763940923,-0.0369432463290883,
0.544730751983338));
#15511=CARTESIAN_POINT('Ctrl Pts',(0.116420979124965,0.112253095453589,
0.552669741620643));
#15512=CARTESIAN_POINT('Ctrl Pts',(-0.0311812332291155,0.158689421555565,
0.56060873125795));
#15513=CARTESIAN_POINT('Ctrl Pts',(-0.150239163551416,0.0598564579197502,
0.568547720895255));
#15514=CARTESIAN_POINT('Ctrl Pts',(-0.131763436204723,-0.0937709907106254,
0.576486710532561));
#15515=CARTESIAN_POINT('Ctrl Pts',(0.00733268664935855,-0.161557523891122,
0.584425700169866));
#15516=CARTESIAN_POINT('Ctrl Pts',(0.139716237417787,-0.0814492162095161,
0.592364689807173));
#15517=CARTESIAN_POINT('Ctrl Pts',(0.144199148209332,0.0732202668325601,
0.600303679444478));
#15518=CARTESIAN_POINT('Ctrl Pts',(0.0166776214282734,0.160861613702037,
0.608242669081784));
#15519=CARTESIAN_POINT('Ctrl Pts',(-0.126111124778327,0.101245177793678,
0.616181658719089));
#15520=CARTESIAN_POINT('Ctrl Pts',(-0.153453779210204,-0.0510542795996006,
0.624120648356396));
#15521=CARTESIAN_POINT('Ctrl Pts',(-0.0403200156494649,-0.156617042997737,
0.6320596379937));
#15522=CARTESIAN_POINT('Ctrl Pts',(0.10972395892722,-0.118807637198397,
0.639998627631007));
#15523=CARTESIAN_POINT('Ctrl Pts',(0.159323168980049,0.0277620180369333,
0.647937617268312));
#15524=CARTESIAN_POINT('Ctrl Pts',(0.0630729369615192,0.148917448414806,
0.655876606905618));
#15525=CARTESIAN_POINT('Ctrl Pts',(-0.0909162461746061,0.133749160748195,
0.663815596542924));
#15526=CARTESIAN_POINT('Ctrl Pts',(-0.161677836835157,-0.00385731715476066,
0.671754586180229));
#15527=CARTESIAN_POINT('Ctrl Pts',(-0.0844344483789265,-0.137932685561743,
0.679693575817536));
#15528=CARTESIAN_POINT('Ctrl Pts',(0.0701028908975481,-0.145740133481257,
0.687632565454841));
#15529=CARTESIAN_POINT('Ctrl Pts',(0.1604658380222,-0.0201324774223393,
0.695571555092147));
#15530=CARTESIAN_POINT('Ctrl Pts',(0.10393330787963,0.123905081947942,0.703510544729453));
#15531=CARTESIAN_POINT('Ctrl Pts',(-0.0477430426119635,0.15451603056473,
0.711449534366758));
#15532=CARTESIAN_POINT('Ctrl Pts',(-0.155713909636705,0.0436781428746717,
0.719388524004064));
#15533=CARTESIAN_POINT('Ctrl Pts',(-0.121139364160222,-0.10714409115852,
0.72732751364137));
#15534=CARTESIAN_POINT('Ctrl Pts',(0.0243299669821161,-0.159883252800214,
0.735266503278675));
#15535=CARTESIAN_POINT('Ctrl Pts',(0.147526880793862,-0.0662602540182413,
0.743205492915981));
#15536=CARTESIAN_POINT('Ctrl Pts',(0.135673045916277,0.0880194662056535,
0.751144482553287));
#15537=CARTESIAN_POINT('Ctrl Pts',(-0.000380164216571841,0.161723397486253,
0.759083472190592));
#15538=CARTESIAN_POINT('Ctrl Pts',(-0.136085360063504,0.0873806419964673,
0.767022461827899));
#15539=CARTESIAN_POINT('Ctrl Pts',(-0.147213735311121,-0.0669531026545853,
0.774961451465203));
#15540=CARTESIAN_POINT('Ctrl Pts',(-0.023578025097595,-0.159995870421162,
0.78290044110251));
#15541=CARTESIAN_POINT('Ctrl Pts',(0.121641751185188,-0.106573384050283,
0.790839430739816));
#15542=CARTESIAN_POINT('Ctrl Pts',(0.155506840911589,0.0444097314676148,
0.798778420377121));
#15543=CARTESIAN_POINT('Ctrl Pts',(0.047016075363265,0.15473878142458,0.806717410014428));
#15544=CARTESIAN_POINT('Ctrl Pts',(-0.104514684958047,0.123415081928621,
0.814656399651731));
#15545=CARTESIAN_POINT('Ctrl Pts',(-0.16036941405942,-0.020886666885039,
0.82259538928904));
#15546=CARTESIAN_POINT('Ctrl Pts',(-0.0694169354231278,-0.146068103622213,
0.830534378926343));
#15547=CARTESIAN_POINT('Ctrl Pts',(0.085081990139753,-0.137534202194171,
0.838473368563651));
#15548=CARTESIAN_POINT('Ctrl Pts',(0.161694184779289,-0.00309716449182502,
0.846412358200955));
#15549=CARTESIAN_POINT('Ctrl Pts',(0.0902864348795877,0.134175115040242,
0.854351347838261));
#15550=CARTESIAN_POINT('Ctrl Pts',(-0.0637723584188847,0.148619272374149,
0.862290337475567));
#15551=CARTESIAN_POINT('Ctrl Pts',(-0.159451928190027,0.0270126713934565,
0.870229327112872));
#15552=CARTESIAN_POINT('Ctrl Pts',(-0.109164185657521,-0.119322178948671,
0.878168316750179));
#15553=CARTESIAN_POINT('Ctrl Pts',(0.0410558873341998,-0.156425752146281,
0.886107306387484));
#15554=CARTESIAN_POINT('Ctrl Pts',(0.153692109215179,-0.0503322698109037,
0.894046296024789));
#15555=CARTESIAN_POINT('Ctrl Pts',(0.125633738317809,0.101836956040625,
0.901985285662096));
#15556=CARTESIAN_POINT('Ctrl Pts',(-0.0174337097671096,0.160781427979367,
0.909924275299401));
#15557=CARTESIAN_POINT('Ctrl Pts',(-0.144541791370401,0.072541521673891,
0.917863264936708));
#15558=CARTESIAN_POINT('Ctrl Pts',(-0.13933176907,-0.082105176128868,0.925802254574012));
#15559=CARTESIAN_POINT('Ctrl Pts',(-0.00657306121577474,-0.161590212220858,
0.933741244211319));
#15560=CARTESIAN_POINT('Ctrl Pts',(0.132202833700187,-0.0931504835251481,
0.941680233848624));
#15561=CARTESIAN_POINT('Ctrl Pts',(0.149956094815541,0.0605621288182698,
0.949619223485929));
#15562=CARTESIAN_POINT('Ctrl Pts',(0.0304348282896272,0.158834262822317,
0.957558213123236));
#15563=CARTESIAN_POINT('Ctrl Pts',(-0.116947437700435,0.111704514835484,
0.965497202760542));
#15564=CARTESIAN_POINT('Ctrl Pts',(-0.157272339407096,-0.0376830608728604,
0.973436192397847));
#15565=CARTESIAN_POINT('Ctrl Pts',(-0.0536251929639052,-0.152574376940928,
0.981375182035153));
#15566=CARTESIAN_POINT('Ctrl Pts',(0.0991121424632477,-0.127794307524525,
0.989314171672459));
#15567=CARTESIAN_POINT('Ctrl Pts',(0.161119104064031,0.0139726921146952,
0.997253161309763));
#15568=CARTESIAN_POINT('Ctrl Pts',(0.0756325681075411,0.142948649734045,
1.00519215094707));
#15569=CARTESIAN_POINT('Ctrl Pts',(-0.0790904005129918,0.141064915432658,
1.01313114058437));
#15570=CARTESIAN_POINT('Ctrl Pts',(-0.161411527883023,0.0100459188627121,
1.02107013022168));
#15571=CARTESIAN_POINT('Ctrl Pts',(-0.095971463730607,-0.130169427934261,
1.02900911985899));
#15572=CARTESIAN_POINT('Ctrl Pts',(0.0573238981132153,-0.151223584550935,
1.03694810949629));
#15573=CARTESIAN_POINT('Ctrl Pts',(0.158143159897702,-0.0338429135403315,
1.0448870991336));
#15574=CARTESIAN_POINT('Ctrl Pts',(0.114193197054413,0.114518625410106,
1.0528260887709));
#15575=CARTESIAN_POINT('Ctrl Pts',(-0.0342928115212847,0.158046211271557,
1.06076507840821));
#15576=CARTESIAN_POINT('Ctrl Pts',(-0.151386101389109,0.0568933223281485,
1.06870406804552));
#15577=CARTESIAN_POINT('Ctrl Pts',(-0.129895790602315,-0.0963415040526547,
1.07664305768282));
#15578=CARTESIAN_POINT('Ctrl Pts',(0.0105052141409744,-0.161382286187737,
1.08458204732013));
#15579=CARTESIAN_POINT('Ctrl Pts',(0.141289415307547,-0.0786886455683398,
1.09252103695743));
#15580=CARTESIAN_POINT('Ctrl Pts',(0.14273283995608,0.076039057183793,1.10046002659474));
#15581=CARTESIAN_POINT('Ctrl Pts',(0.013514131745196,0.161158214381091,
1.10839901623204));
#15582=CARTESIAN_POINT('Ctrl Pts',(-0.128075837894479,0.0987480712062529,
1.11633800586935));
#15583=CARTESIAN_POINT('Ctrl Pts',(-0.152421155552179,-0.0540591635106084,
1.12427699550666));
#15584=CARTESIAN_POINT('Ctrl Pts',(-0.0372353514058616,-0.157378938949945,
1.13221598514396));
#15585=CARTESIAN_POINT('Ctrl Pts',(0.11203686504723,-0.116629081663695,
1.14015497478127));
#15586=CARTESIAN_POINT('Ctrl Pts',(0.158747009937404,0.0308867067726846,
1.14809396441857));
#15587=CARTESIAN_POINT('Ctrl Pts',(0.0601351468730053,0.150127831962932,
1.15603295405588));
#15588=CARTESIAN_POINT('Ctrl Pts',(-0.0935263218228598,0.13193721592339,
1.16397194369318));
#15589=CARTESIAN_POINT('Ctrl Pts',(-0.161570852667341,-0.00703287904607843,
1.17191093333049));
#15590=CARTESIAN_POINT('Ctrl Pts',(-0.0817083410685703,-0.13956485524354,
1.17984992296779));
#15591=CARTESIAN_POINT('Ctrl Pts',(0.0729525569401478,-0.144334771469742,
1.1877889126051));
#15592=CARTESIAN_POINT('Ctrl Pts',(0.160830388835411,-0.016976096323307,
1.19572790224241));
#15593=CARTESIAN_POINT('Ctrl Pts',(0.101479022178261,0.125923031559255,
1.20366689187971));
#15594=CARTESIAN_POINT('Ctrl Pts',(-0.0507694344715009,0.153548254118279,
1.21160588151702));
#15595=CARTESIAN_POINT('Ctrl Pts',(-0.15654195331917,0.0406105733811438,
1.21954487115432));
#15596=CARTESIAN_POINT('Ctrl Pts',(-0.119011042423884,-0.109503304062093,
1.22748386079163));
#15597=CARTESIAN_POINT('Ctrl Pts',(0.0274663214511058,-0.159374411387982,
1.23542285042894));
#15598=CARTESIAN_POINT('Ctrl Pts',(0.148800150427453,-0.0633491677300162,
1.24336184006624));
#15599=CARTESIAN_POINT('Ctrl Pts',(0.133917639627974,0.0906678973829495,
1.25130082970354));
#15600=CARTESIAN_POINT('Ctrl Pts',(-0.00355729227603857,0.161684716318317,
1.25923981934086));
#15601=CARTESIAN_POINT('Ctrl Pts',(-0.137775766897813,0.0846902584421788,
1.26717880897816));
#15602=CARTESIAN_POINT('Ctrl Pts',(-0.14586996931591,-0.0698323268364953,
1.27511779861547));
#15603=CARTESIAN_POINT('Ctrl Pts',(-0.0204302119447119,-0.160428202816007,
1.28305678825277));
#15604=CARTESIAN_POINT('Ctrl Pts',(0.123712004283314,-0.104163053984564,
1.29099577789008));
#15605=CARTESIAN_POINT('Ctrl Pts',(0.15460435913624,0.0474562320176185,
1.29893476752738));
#15606=CARTESIAN_POINT('Ctrl Pts',(0.043967018911749,0.155632589980133,
1.30687375716469));
#15607=CARTESIAN_POINT('Ctrl Pts',(-0.106919113837756,0.121337978043289,
1.31481274680199));
#15608=CARTESIAN_POINT('Ctrl Pts',(-0.159928125575155,-0.0240332370134145,
1.3227517364393));
#15609=CARTESIAN_POINT('Ctrl Pts',(-0.0665338988230771,-0.147403670583407,
1.33069072607661));
#15610=CARTESIAN_POINT('Ctrl Pts',(0.0877675522160205,-0.135836146169277,
1.33862971571391));
#15611=CARTESIAN_POINT('Ctrl Pts',(0.161723824721502,8.00609866524728E-5,
1.34656870535122));
#15612=CARTESIAN_POINT('Ctrl Pts',(0.0876330185603928,0.135922977069285,
1.35450769498852));
#15613=CARTESIAN_POINT('Ctrl Pts',(-0.0666798087068602,0.147337724435113,
1.36244668462583));
#15614=CARTESIAN_POINT('Ctrl Pts',(-0.159951843822013,0.0238748801740983,
1.37038567426313));
#15615=CARTESIAN_POINT('Ctrl Pts',(-0.106798922716859,-0.121443775659372,
1.37832466390044));
#15616=CARTESIAN_POINT('Ctrl Pts',(0.0441210824430389,-0.155588987406456,
1.38626365353774));
#15617=CARTESIAN_POINT('Ctrl Pts',(0.154651279966657,-0.0473031264624986,
1.39420264317505));
#15618=CARTESIAN_POINT('Ctrl Pts',(0.123608792556459,0.10428547082216,1.40214163281236));
#15619=CARTESIAN_POINT('Ctrl Pts',(-0.020589002599541,0.160407931346284,
1.41008062244966));
#15620=CARTESIAN_POINT('Ctrl Pts',(-0.145939110542184,0.0696878015005003,
1.41801961208697));
#15621=CARTESIAN_POINT('Ctrl Pts',(-0.137691710982408,-0.0848265016612731,
1.42595860172427));
#15622=CARTESIAN_POINT('Ctrl Pts',(-0.00339746822928561,-0.161688398335044,
1.43389759136158));
#15623=CARTESIAN_POINT('Ctrl Pts',(0.134007838137522,-0.0905348079547059,
1.44183658099889));
#15624=CARTESIAN_POINT('Ctrl Pts',(0.148736417039967,0.0634956003383226,
1.44977557063619));
#15625=CARTESIAN_POINT('Ctrl Pts',(0.0273102951854726,0.159403164432859,
1.4577145602735));
#15626=CARTESIAN_POINT('Ctrl Pts',(-0.119122786779006,0.109382310628272,
1.4656535499108));
#15627=CARTESIAN_POINT('Ctrl Pts',(-0.156495242883694,-0.0407596439572756,
1.47359253954811));
#15628=CARTESIAN_POINT('Ctrl Pts',(-0.0506295842364637,-0.153609649276743,
1.48153152918541));
#15629=CARTESIAN_POINT('Ctrl Pts',(0.10162683549218,-0.125801210382132,
1.48947051882272));
#15630=CARTESIAN_POINT('Ctrl Pts',(0.160769288057966,0.017094787472962,
1.49740950846002));
#15631=CARTESIAN_POINT('Ctrl Pts',(0.0728951834924312,0.144484958595688,
1.50534849809733));
#15632=CARTESIAN_POINT('Ctrl Pts',(-0.0820226078184241,0.139326700971572,
1.51328748773464));
#15633=CARTESIAN_POINT('Ctrl Pts',(-0.134767702434085,0.0512744806661359,
1.51858014749284));
#15634=CARTESIAN_POINT('Ctrl Pts',(-0.136701386950156,0.00581475974600206,
1.52122647737194));
#15635=CARTESIAN_POINT('Ctrl Pts',(0.0740036351041134,-0.103579689087085,
-0.0054992613140312));
#15636=CARTESIAN_POINT('Ctrl Pts',(0.108448814220036,-0.0789699563406641,
-0.00285293143492929));
#15637=CARTESIAN_POINT('Ctrl Pts',(0.150264871169078,0.00688399744800666,
0.00243972832327453));
#15638=CARTESIAN_POINT('Ctrl Pts',(0.0755551489391376,0.130236700260234,
0.0103787179605803));
#15639=CARTESIAN_POINT('Ctrl Pts',(-0.0683810376584167,0.133979098529349,
0.0183177075978859));
#15640=CARTESIAN_POINT('Ctrl Pts',(-0.14968704878538,0.0152677557027674,
0.0262566972351917));
#15641=CARTESIAN_POINT('Ctrl Pts',(-0.0939816891590436,-0.11752176362514,
0.0341956868724974));
#15642=CARTESIAN_POINT('Ctrl Pts',(0.0477663481097245,-0.142674779628989,
0.0421346765098031));
#15643=CARTESIAN_POINT('Ctrl Pts',(0.14578288888032,-0.0372469160898187,
0.0500736661471088));
#15644=CARTESIAN_POINT('Ctrl Pts',(0.110347650287512,0.102292747252513,
0.0580126557844146));
#15645=CARTESIAN_POINT('Ctrl Pts',(-0.0261045975097209,0.148182615303324,
0.0659516454217203));
#15646=CARTESIAN_POINT('Ctrl Pts',(-0.13865919166998,0.0584255608647477,
0.073890635059026));
#15647=CARTESIAN_POINT('Ctrl Pts',(-0.124281158904105,-0.0848182532198701,
0.0818296246963318));
#15648=CARTESIAN_POINT('Ctrl Pts',(0.00386794697500161,-0.15041563023346,
0.0897686143336374));
#15649=CARTESIAN_POINT('Ctrl Pts',(0.128476112576568,-0.0783184064825255,
0.0977076039709433));
#15650=CARTESIAN_POINT('Ctrl Pts',(0.135473254782295,0.0654742669580799,
0.105646593608249));
#15651=CARTESIAN_POINT('Ctrl Pts',(0.0184538891044151,0.149329569763132,
0.113585583245555));
#15652=CARTESIAN_POINT('Ctrl Pts',(-0.115458732720671,0.096483973363118,
0.12152457288286));
#15653=CARTESIAN_POINT('Ctrl Pts',(-0.143676805334049,-0.0446861343604874,
0.129463562520166));
#15654=CARTESIAN_POINT('Ctrl Pts',(-0.0403686054279526,-0.144949124289353,
0.137402552157472));
#15655=CARTESIAN_POINT('Ctrl Pts',(0.0998942839726139,-0.112521137758025,
0.145341541794778));
#15656=CARTESIAN_POINT('Ctrl Pts',(0.14871080372247,0.0229122455632766,
0.153280531432083));
#15657=CARTESIAN_POINT('Ctrl Pts',(0.0613927738894439,0.137371034794898,
0.161219521069389));
#15658=CARTESIAN_POINT('Ctrl Pts',(-0.0821261326059948,0.126076058196294,
0.169158510706695));
#15659=CARTESIAN_POINT('Ctrl Pts',(-0.150464193336327,-0.000632910110818063,
0.177097500344));
#15660=CARTESIAN_POINT('Ctrl Pts',(-0.0810625969653723,-0.126762492068094,
0.185036489981306));
#15661=CARTESIAN_POINT('Ctrl Pts',(0.0625462512992226,-0.136849700411639,
0.192975479618612));
#15662=CARTESIAN_POINT('Ctrl Pts',(0.148898293097928,-0.0216603868066741,
0.200914469255917));
#15663=CARTESIAN_POINT('Ctrl Pts',(0.0989441522193119,0.113357526360621,
0.208853458893223));
#15664=CARTESIAN_POINT('Ctrl Pts',(-0.0415865789238149,0.144604393083411,
0.216792448530529));
#15665=CARTESIAN_POINT('Ctrl Pts',(-0.144047647180085,0.0434758483035601,
0.224731438167835));
#15666=CARTESIAN_POINT('Ctrl Pts',(-0.114642966671137,-0.0974518559926297,
0.232670427805141));
#15667=CARTESIAN_POINT('Ctrl Pts',(0.0197094928286333,-0.149169064945282,
0.240609417442446));
#15668=CARTESIAN_POINT('Ctrl Pts',(0.136019262424063,-0.0643322181611298,
0.248548407079752));
#15669=CARTESIAN_POINT('Ctrl Pts',(0.127812719278849,0.0793963653730636,
0.256487396717058));
#15670=CARTESIAN_POINT('Ctrl Pts',(0.00260239121171357,0.150443017797356,
0.264426386354363));
#15671=CARTESIAN_POINT('Ctrl Pts',(-0.124990247656303,0.0837693979610897,
0.272365375991669));
#15672=CARTESIAN_POINT('Ctrl Pts',(-0.138162880936044,-0.0595893646165358,
0.280304365628975));
#15673=CARTESIAN_POINT('Ctrl Pts',(-0.0248568656394851,-0.148398147813718,
0.288243355266281));
#15674=CARTESIAN_POINT('Ctrl Pts',(0.111203906597776,-0.101358597076653,
0.296182344903586));
#15675=CARTESIAN_POINT('Ctrl Pts',(0.145465123646218,0.0384678027257296,
0.304121334540892));
#15676=CARTESIAN_POINT('Ctrl Pts',(0.0465629893725541,0.143079565503422,
0.312060324178198));
#15677=CARTESIAN_POINT('Ctrl Pts',(-0.0949643705016135,0.116711791945748,
0.319999313815503));
#15678=CARTESIAN_POINT('Ctrl Pts',(-0.149558357514911,-0.0164976283567656,
0.327938303452809));
#15679=CARTESIAN_POINT('Ctrl Pts',(-0.0672419181269484,-0.134604600554976,
0.335877293090115));
#15680=CARTESIAN_POINT('Ctrl Pts',(0.0766298889166206,-0.12949028600085,
0.343816282727421));
#15681=CARTESIAN_POINT('Ctrl Pts',(0.150352284446295,-0.00583648916182633,
0.351755272364726));
#15682=CARTESIAN_POINT('Ctrl Pts',(0.0864374678803939,0.123160213504125,
0.359694262002032));
#15683=CARTESIAN_POINT('Ctrl Pts',(-0.0566049265834532,0.139412181427728,
0.367633251639338));
#15684=CARTESIAN_POINT('Ctrl Pts',(-0.147829390149123,0.0280418517950267,
0.375572241276644));
#15685=CARTESIAN_POINT('Ctrl Pts',(-0.103726178443039,-0.108998871322406,
0.383511230913949));
#15686=CARTESIAN_POINT('Ctrl Pts',(0.0353312408083745,-0.146258597924691,
0.391450220551255));
#15687=CARTESIAN_POINT('Ctrl Pts',(0.142045330507792,-0.0496286018832686,
0.399389210188561));
#15688=CARTESIAN_POINT('Ctrl Pts',(0.118726655129599,0.0924329779120693,
0.407328199825866));
#15689=CARTESIAN_POINT('Ctrl Pts',(-0.0132781361506635,0.1498785012746,
0.415267189463172));
#15690=CARTESIAN_POINT('Ctrl Pts',(-0.133127703795094,0.0701205285647604,
0.423206179100478));
#15691=CARTESIAN_POINT('Ctrl Pts',(-0.131107982452518,-0.0738279823724454,
0.431145168737783));
#15692=CARTESIAN_POINT('Ctrl Pts',(-0.00906788859151817,-0.150192035209753,
0.439084158375089));
#15693=CARTESIAN_POINT('Ctrl Pts',(0.121273235812024,-0.0890655731449414,
0.447023148012395));
#15694=CARTESIAN_POINT('Ctrl Pts',(0.14059702422731,0.0535943170716914,
0.4549621376497));
#15695=CARTESIAN_POINT('Ctrl Pts',(0.031213872705855,0.14719228306762,0.462901127287006));
#15696=CARTESIAN_POINT('Ctrl Pts',(-0.106743440051405,0.106045801661112,
0.470840116924312));
#15697=CARTESIAN_POINT('Ctrl Pts',(-0.146984449047318,-0.0321783433727119,
0.478779106561618));
#15698=CARTESIAN_POINT('Ctrl Pts',(-0.0526712684425847,-0.140945420374714,
0.486718096198923));
#15699=CARTESIAN_POINT('Ctrl Pts',(0.0898588486235595,-0.120686624644175,
0.49465708583623));
#15700=CARTESIAN_POINT('Ctrl Pts',(0.150129348203927,0.0100525047535443,
0.502596075473534));
#15701=CARTESIAN_POINT('Ctrl Pts',(0.0729667185397875,0.131589254992538,
0.510535065110842));
#15702=CARTESIAN_POINT('Ctrl Pts',(-0.0709919412117167,0.132665060686482,
0.518474054748145));
#15703=CARTESIAN_POINT('Ctrl Pts',(-0.149962344179375,0.0122950954523496,
0.526413044385453));
#15704=CARTESIAN_POINT('Ctrl Pts',(-0.0916524986414713,-0.119330187030486,
0.534352034022757));
#15705=CARTESIAN_POINT('Ctrl Pts',(0.0505589280467443,-0.141716861518734,
0.542291023660064));
#15706=CARTESIAN_POINT('Ctrl Pts',(0.146487121137799,-0.0343714617774037,
0.550230013297369));
#15707=CARTESIAN_POINT('Ctrl Pts',(0.108316394245265,0.104438655591022,
0.558169002934674));
#15708=CARTESIAN_POINT('Ctrl Pts',(-0.0290105681715044,0.147642341414387,
0.566107992571982));
#15709=CARTESIAN_POINT('Ctrl Pts',(-0.139780343651344,0.0556895822633619,
0.574046982209285));
#15710=CARTESIAN_POINT('Ctrl Pts',(-0.122590794290966,-0.0872431727934394,
0.581985971846593));
#15711=CARTESIAN_POINT('Ctrl Pts',(0.00682222554696161,-0.150310782322966,
0.589924961483898));
#15712=CARTESIAN_POINT('Ctrl Pts',(0.129989965454297,-0.0757791721064987,
0.597863951121203));
#15713=CARTESIAN_POINT('Ctrl Pts',(0.134160800782372,0.0681230766876274,
0.60580294075851));
#15714=CARTESIAN_POINT('Ctrl Pts',(0.015516617634347,0.149663317553585,
0.613741930395814));
#15715=CARTESIAN_POINT('Ctrl Pts',(-0.117331965534667,0.0941970482962578,
0.621680920033121));
#15716=CARTESIAN_POINT('Ctrl Pts',(-0.142771175541451,-0.0475001629309618,
0.629619909670426));
#15717=CARTESIAN_POINT('Ctrl Pts',(-0.0375131590877193,-0.145714230393655,
0.637558899307733));
#15718=CARTESIAN_POINT('Ctrl Pts',(0.102085583566124,-0.110536906379362,
0.645497888945037));
#15719=CARTESIAN_POINT('Ctrl Pts',(0.148231970847143,0.0258293798362968,
0.653436878582344));
#15720=CARTESIAN_POINT('Ctrl Pts',(0.0586821478180281,0.138550639014834,
0.661375868219649));
#15721=CARTESIAN_POINT('Ctrl Pts',(-0.0845871597882484,0.124438283670714,
0.669314857856955));
#15722=CARTESIAN_POINT('Ctrl Pts',(-0.150422719745043,-0.00358879206139753,
0.67725384749426));
#15723=CARTESIAN_POINT('Ctrl Pts',(-0.078556588917505,-0.128330574617282,
0.685192837131567));
#15724=CARTESIAN_POINT('Ctrl Pts',(0.065222715229363,-0.135594511179713,
0.693131826768872));
#15725=CARTESIAN_POINT('Ctrl Pts',(0.149295093588351,-0.0187309656558678,
0.701070816406178));
#15726=CARTESIAN_POINT('Ctrl Pts',(0.0966980456281902,0.11527949520901,
0.709009806043483));
#15727=CARTESIAN_POINT('Ctrl Pts',(-0.044419435954706,0.14375947882982,
0.716948795680789));
#15728=CARTESIAN_POINT('Ctrl Pts',(-0.144873968183829,0.0406375120624596,
0.724887785318095));
#15729=CARTESIAN_POINT('Ctrl Pts',(-0.112706311402131,-0.099685311927494,
0.732826774955401));
#15730=CARTESIAN_POINT('Ctrl Pts',(0.0226362492002416,-0.148753064728429,
0.740765764592706));
#15731=CARTESIAN_POINT('Ctrl Pts',(0.137256875023267,-0.0616475814838108,
0.748704754230013));
#15732=CARTESIAN_POINT('Ctrl Pts',(0.126228238590478,0.0818920376245527,
0.756643743867318));
#15733=CARTESIAN_POINT('Ctrl Pts',(-0.000353699285724532,0.150465108715513,
0.764582733504624));
#15734=CARTESIAN_POINT('Ctrl Pts',(-0.126611849706441,0.0812976848247803,
0.772521723141928));
#15735=CARTESIAN_POINT('Ctrl Pts',(-0.136965528997667,-0.0622921978288208,
0.780460712779236));
#15736=CARTESIAN_POINT('Ctrl Pts',(-0.0219366533522686,-0.148857842533265,
0.788399702416541));
#15737=CARTESIAN_POINT('Ctrl Pts',(0.113173725020093,-0.0991543342927188,
0.796338692053846));
#15738=CARTESIAN_POINT('Ctrl Pts',(0.144681314438483,0.0413181715024817,
0.804277681691154));
#15739=CARTESIAN_POINT('Ctrl Pts',(0.0437430761464933,0.143966723006387,
0.812216671328456));
#15740=CARTESIAN_POINT('Ctrl Pts',(-0.0972389504488157,0.114823606281847,
0.820155660965765));
#15741=CARTESIAN_POINT('Ctrl Pts',(-0.149205382128735,-0.0194326526180533,
0.828094650603069));
#15742=CARTESIAN_POINT('Ctrl Pts',(-0.0645845121824554,-0.135899649852787,
0.836033640240376));
#15743=CARTESIAN_POINT('Ctrl Pts',(0.0791590524011713,-0.127959831458565,
0.843972629877681));
#15744=CARTESIAN_POINT('Ctrl Pts',(0.150437929635691,-0.00288155702400619,
0.851911619514986));
#15745=CARTESIAN_POINT('Ctrl Pts',(0.0840011924733913,0.12483458538003,
0.859850609152293));
#15746=CARTESIAN_POINT('Ctrl Pts',(-0.0593328794206009,0.138273220341526,
0.867789598789597));
#15747=CARTESIAN_POINT('Ctrl Pts',(-0.148351766552825,0.0251321985630355,
0.875728588426904));
#15748=CARTESIAN_POINT('Ctrl Pts',(-0.1015647786165,-0.111015628577859,
0.883667578064211));
#15749=CARTESIAN_POINT('Ctrl Pts',(0.0381978034543637,-0.145536256153639,
0.891606567701514));
#15750=CARTESIAN_POINT('Ctrl Pts',(0.142992914329196,-0.046828415471795,
0.899545557338823));
#15751=CARTESIAN_POINT('Ctrl Pts',(0.116887812080083,0.0947476302135675,
0.907484546976125));
#15752=CARTESIAN_POINT('Ctrl Pts',(-0.0162200712834111,0.149588713917584,
0.915423536613434));
#15753=CARTESIAN_POINT('Ctrl Pts',(-0.134479591021026,0.067491582014154,
0.923362526250738));
#15754=CARTESIAN_POINT('Ctrl Pts',(-0.129632261667175,-0.0763894677230377,
0.931301515888044));
#15755=CARTESIAN_POINT('Ctrl Pts',(-0.00611548103612966,-0.150341195071919,
0.93924050552535));
#15756=CARTESIAN_POINT('Ctrl Pts',(0.122999603362204,-0.0866658618874593,
0.947179495162656));
#15757=CARTESIAN_POINT('Ctrl Pts',(0.139516980595786,0.0563461282555487,
0.95511848479996));
#15758=CARTESIAN_POINT('Ctrl Pts',(0.0283161238170646,0.147777099632969,
0.963057474437267));
#15759=CARTESIAN_POINT('Ctrl Pts',(-0.108806203685475,0.103928264122473,
0.970996464074573));
#15760=CARTESIAN_POINT('Ctrl Pts',(-0.146323908690103,-0.0350597745230392,
0.978935453711877));
#15761=CARTESIAN_POINT('Ctrl Pts',(-0.049892103521326,-0.14195299239598,
0.986874443349185));
#15762=CARTESIAN_POINT('Ctrl Pts',(0.0922125030920605,-0.118897974404329,
0.994813432986488));
#15763=CARTESIAN_POINT('Ctrl Pts',(0.149902882860231,0.0129999905441286,
1.0027524226238));
#15764=CARTESIAN_POINT('Ctrl Pts',(0.0703674468853664,0.132997355096976,
1.0106914122611));
#15765=CARTESIAN_POINT('Ctrl Pts',(-0.0735845641169637,0.131244755962562,
1.01863040189841));
#15766=CARTESIAN_POINT('Ctrl Pts',(-0.150174949749745,0.00934657753497952,
1.02656939153571));
#15767=CARTESIAN_POINT('Ctrl Pts',(-0.0892904610481016,-0.121107752063083,
1.03450838117302));
#15768=CARTESIAN_POINT('Ctrl Pts',(0.0533333252681307,-0.140696234703703,
1.04244737081032));
#15769=CARTESIAN_POINT('Ctrl Pts',(0.147134107472884,-0.031486957015783,
1.05038636044763));
#15770=CARTESIAN_POINT('Ctrl Pts',(0.106243698045146,0.106546471877992,
1.05832535008494));
#15771=CARTESIAN_POINT('Ctrl Pts',(-0.0319055355867657,0.147043907874068,
1.06626433972224));
#15772=CARTESIAN_POINT('Ctrl Pts',(-0.14084743801815,0.0529327237885883,
1.07420332935955));
#15773=CARTESIAN_POINT('Ctrl Pts',(-0.120853163849259,-0.0896347412088629,
1.08214231899685));
#15774=CARTESIAN_POINT('Ctrl Pts',(0.00977389921538986,-0.150147743699608,
1.09008130863416));
#15775=CARTESIAN_POINT('Ctrl Pts',(0.13145362739741,-0.0732107771302755,
1.09802029827146));
#15776=CARTESIAN_POINT('Ctrl Pts',(0.132796568802552,0.0707456384395876,
1.10595928790877));
#15777=CARTESIAN_POINT('Ctrl Pts',(0.0125733526121963,0.149939270533256,
1.11389827754607));
#15778=CARTESIAN_POINT('Ctrl Pts',(-0.119159906186493,0.0918737764630459,
1.12183726718338));
#15779=CARTESIAN_POINT('Ctrl Pts',(-0.141810437433163,-0.0502958634379693,
1.12977625682069));
#15780=CARTESIAN_POINT('Ctrl Pts',(-0.0346432321137694,-0.146423087362162,
1.13771524645799));
#15781=CARTESIAN_POINT('Ctrl Pts',(0.104237477950025,-0.108510009835838,
1.1456542360953));
#15782=CARTESIAN_POINT('Ctrl Pts',(0.147695920811486,0.0287365450185451,
1.1535932257326));
#15783=CARTESIAN_POINT('Ctrl Pts',(0.0559488704325515,0.139676762352502,
1.16153221536991));
#15784=CARTESIAN_POINT('Ctrl Pts',(-0.0870155364008756,0.12275247642644,
1.16947120500722));
#15785=CARTESIAN_POINT('Ctrl Pts',(-0.150323183223479,-0.00654328889139735,
1.17741019464452));
#15786=CARTESIAN_POINT('Ctrl Pts',(-0.0760202581255566,-0.129849121670035,
1.18534918428183));
#15787=CARTESIAN_POINT('Ctrl Pts',(0.0678740032777675,-0.134286982701248,
1.19328817391913));
#15788=CARTESIAN_POINT('Ctrl Pts',(0.149634266389533,-0.0157943143574443,
1.20122716355644));
#15789=CARTESIAN_POINT('Ctrl Pts',(0.0944146137277022,0.117156966325547,
1.20916615319374));
#15790=CARTESIAN_POINT('Ctrl Pts',(-0.047235147145783,0.142859073628774,
1.21710514283105));
#15791=CARTESIAN_POINT('Ctrl Pts',(-0.145644368043342,0.037783489796601,
1.22504413246835));
#15792=CARTESIAN_POINT('Ctrl Pts',(-0.11072615165767,-0.101880289472715,
1.23298312210566));
#15793=CARTESIAN_POINT('Ctrl Pts',(0.0255542680118797,-0.148279646041953,
1.24092211174296));
#15794=CARTESIAN_POINT('Ctrl Pts',(0.138441506664824,-0.0589391489276913,
1.24886110138027));
#15795=CARTESIAN_POINT('Ctrl Pts',(0.124595033982396,0.0843560996663564,
1.25680009101758));
#15796=CARTESIAN_POINT('Ctrl Pts',(-0.00330965325590636,0.150429120316621,
1.26473908065488));
#15797=CARTESIAN_POINT('Ctrl Pts',(-0.128184579763139,0.0787945908985174,
1.27267807029219));
#15798=CARTESIAN_POINT('Ctrl Pts',(-0.135715308561414,-0.0649709863423027,
1.2806170599295));
#15799=CARTESIAN_POINT('Ctrl Pts',(-0.0190079735469551,-0.149260078337129,
1.2885560495668));
#15800=CARTESIAN_POINT('Ctrl Pts',(0.115099858543875,-0.0969117980795561,
1.29649503920411));
#15801=CARTESIAN_POINT('Ctrl Pts',(0.143841658454547,0.0441525915281748,
1.30443402884141));
#15802=CARTESIAN_POINT('Ctrl Pts',(0.0409062781470196,0.144798309552134,
1.31237301847872));
#15803=CARTESIAN_POINT('Ctrl Pts',(-0.0994759962839106,0.112891098884786,
1.32031200811602));
#15804=CARTESIAN_POINT('Ctrl Pts',(-0.148794813708878,-0.0223601759313527,
1.32825099775333));
#15805=CARTESIAN_POINT('Ctrl Pts',(-0.0619021766503053,-0.13714224202644,
1.33618998739064));
#15806=CARTESIAN_POINT('Ctrl Pts',(0.0816576604940555,-0.126379984705639,
1.34412897702794));
#15807=CARTESIAN_POINT('Ctrl Pts',(0.150465506209006,7.4487583413377E-5,
1.35206796666525));
#15808=CARTESIAN_POINT('Ctrl Pts',(0.0815324923277053,0.126460770918471,
1.36000695630255));
#15809=CARTESIAN_POINT('Ctrl Pts',(-0.062037929094705,0.137080886684378,
1.36794594593986));
#15810=CARTESIAN_POINT('Ctrl Pts',(-0.148816880822527,0.0222128430196456,
1.37588493557716));
#15811=CARTESIAN_POINT('Ctrl Pts',(-0.0993641722043223,-0.112989531455785,
1.38382392521447));
#15812=CARTESIAN_POINT('Ctrl Pts',(0.0410496166270677,-0.144757742348562,
1.39176291485178));
#15813=CARTESIAN_POINT('Ctrl Pts',(0.143885312916173,-0.0440101443352923,
1.39970190448908));
#15814=CARTESIAN_POINT('Ctrl Pts',(0.115003831846793,0.0970256929337524,
1.40764089412639));
#15815=CARTESIAN_POINT('Ctrl Pts',(-0.0191557100743377,0.149241218055048,
1.41557988376369));
#15816=CARTESIAN_POINT('Ctrl Pts',(-0.135779636557791,0.0648365220611291,
1.423518873401));
#15817=CARTESIAN_POINT('Ctrl Pts',(-0.128106375355825,-0.0789213496179777,
1.4314578630383));
#15818=CARTESIAN_POINT('Ctrl Pts',(-0.00316095527563228,-0.150432546011701,
1.43939685267561));
#15819=CARTESIAN_POINT('Ctrl Pts',(0.12467895337041,-0.0842322751882648,
1.44733584231291));
#15820=CARTESIAN_POINT('Ctrl Pts',(0.138382210043398,0.0590753877074232,
1.45527483195022));
#15821=CARTESIAN_POINT('Ctrl Pts',(0.0254091034322018,0.148306397458819,
1.46321382158753));
#15822=CARTESIAN_POINT('Ctrl Pts',(-0.110830116988615,0.101767718932792,
1.47115281122483));
#15823=CARTESIAN_POINT('Ctrl Pts',(-0.145600909330124,-0.0379221829034233,
1.47909180086214));
#15824=CARTESIAN_POINT('Ctrl Pts',(-0.0471050325108872,-0.142916194795756,
1.48703079049945));
#15825=CARTESIAN_POINT('Ctrl Pts',(0.0945521370959566,-0.117043625665234,
1.49496978013675));
#15826=CARTESIAN_POINT('Ctrl Pts',(0.14957741911039,0.0159047428854941,
1.50290876977406));
#15827=CARTESIAN_POINT('Ctrl Pts',(0.0678206238522695,0.134426714629862,
1.51084775941136));
#15828=CARTESIAN_POINT('Ctrl Pts',(-0.0763126473618499,0.129627546381738,
1.51878674904867));
#15829=CARTESIAN_POINT('Ctrl Pts',(-0.125385920115907,0.0477050348167321,
1.52407940880687));
#15830=CARTESIAN_POINT('Ctrl Pts',(-0.127184992207234,0.00540996832206346,
1.52672573868597));
#15831=CARTESIAN_POINT('Ctrl Pts',(0.0684664424539414,-0.095829519891843,
-1.38777878078145E-17));
#15832=CARTESIAN_POINT('Ctrl Pts',(0.100334321247169,-0.0730611673843044,
0.00264632987910189));
#15833=CARTESIAN_POINT('Ctrl Pts',(0.139021564822767,0.00636891437108143,
0.00793898963730573));
#15834=CARTESIAN_POINT('Ctrl Pts',(0.0699018669780613,0.120491966796142,
0.0158779792746114));
#15835=CARTESIAN_POINT('Ctrl Pts',(-0.0632645460347191,0.123954346655885,
0.0238169689119172));
#15836=CARTESIAN_POINT('Ctrl Pts',(-0.138486976988987,0.0141253725679007,
0.0317559585492228));
#15837=CARTESIAN_POINT('Ctrl Pts',(-0.0869496735326521,-0.108728403071097,
0.0396949481865287));
#15838=CARTESIAN_POINT('Ctrl Pts',(0.0441923146003338,-0.131999388615902,
0.0476339378238343));
#15839=CARTESIAN_POINT('Ctrl Pts',(0.134874939024977,-0.034459980695041,
0.0555729274611401));
#15840=CARTESIAN_POINT('Ctrl Pts',(0.102091080224759,0.094638871230671,
0.0635119170984456));
#15841=CARTESIAN_POINT('Ctrl Pts',(-0.0241513666277066,0.137095110112719,
0.0714509067357516));
#15842=CARTESIAN_POINT('Ctrl Pts',(-0.128284260007319,0.0540539703915629,
0.0793898963730571));
#15843=CARTESIAN_POINT('Ctrl Pts',(-0.114982038412656,-0.0784718756714057,
0.0873288860103631));
#15844=CARTESIAN_POINT('Ctrl Pts',(0.00357853460314598,-0.139161043603659,
0.0952678756476685));
#15845=CARTESIAN_POINT('Ctrl Pts',(0.118863112008681,-0.0724583686054966,
0.103206865284975));
#15846=CARTESIAN_POINT('Ctrl Pts',(0.125336705278751,0.0605752693714656,
0.11114585492228));
#15847=CARTESIAN_POINT('Ctrl Pts',(0.0170731091066207,0.138156245709763,
0.119084844559586));
#15848=CARTESIAN_POINT('Ctrl Pts',(-0.106819734848208,0.0892647286947484,
0.127023834196891));
#15849=CARTESIAN_POINT('Ctrl Pts',(-0.132926439498961,-0.0413425724611633,
0.134962823834197));
#15850=CARTESIAN_POINT('Ctrl Pts',(-0.0373480950846616,-0.134103559412242,
0.142901813471503));
#15851=CARTESIAN_POINT('Ctrl Pts',(0.0924198687735613,-0.104101940294199,
0.150840803108809));
#15852=CARTESIAN_POINT('Ctrl Pts',(0.137583777756591,0.0211978768359354,
0.158779792746114));
#15853=CARTESIAN_POINT('Ctrl Pts',(0.0567991668878991,0.127092487218924,
0.16671878238342));
#15854=CARTESIAN_POINT('Ctrl Pts',(-0.075981188277068,0.116642637502503,
0.174657772020726));
#15855=CARTESIAN_POINT('Ctrl Pts',(-0.139205973057234,-0.000585553717998882,
0.182596761658032));
#15856=CARTESIAN_POINT('Ctrl Pts',(-0.0749972298318695,-0.11727771015962,
0.190535751295337));
#15857=CARTESIAN_POINT('Ctrl Pts',(0.0578663373665801,-0.126610160769685,
0.198474740932643));
#15858=CARTESIAN_POINT('Ctrl Pts',(0.13775723856723,-0.0200396862227523,
0.206413730569949));
#15859=CARTESIAN_POINT('Ctrl Pts',(0.091540828968026,0.104875747581476,
0.214352720207254));
#15860=CARTESIAN_POINT('Ctrl Pts',(-0.0384749358425138,0.133784622116252,
0.22229170984456));
#15861=CARTESIAN_POINT('Ctrl Pts',(-0.133269533752038,0.0402228439430644,
0.230230699481866));
#15862=CARTESIAN_POINT('Ctrl Pts',(-0.106065007067505,-0.0901601911982067,
0.238169689119172));
#15863=CARTESIAN_POINT('Ctrl Pts',(0.0182347644767634,-0.138007750384372,
0.246108678756477));
#15864=CARTESIAN_POINT('Ctrl Pts',(0.125841858853055,-0.0595186723796334,
0.254047668393783));
#15865=CARTESIAN_POINT('Ctrl Pts',(0.118249355954961,0.073455671106145,
0.261986658031089));
#15866=CARTESIAN_POINT('Ctrl Pts',(0.00240767183786234,0.139186381940956,
0.269925647668394));
#15867=CARTESIAN_POINT('Ctrl Pts',(-0.115638070838342,0.0775014991741366,
0.277864637305701));
#15868=CARTESIAN_POINT('Ctrl Pts',(-0.12782508485658,-0.0551306945617612,
0.285803626943006));
#15869=CARTESIAN_POINT('Ctrl Pts',(-0.0229969941138309,-0.137294515779738,
0.293742616580312));
#15870=CARTESIAN_POINT('Ctrl Pts',(0.102883268653204,-0.0937746172089793,
0.301681606217617));
#15871=CARTESIAN_POINT('Ctrl Pts',(0.134580950019115,0.0355895166223291,
0.309620595854923));
#15872=CARTESIAN_POINT('Ctrl Pts',(0.0430789950773988,0.13237388709478,
0.317559585492229));
#15873=CARTESIAN_POINT('Ctrl Pts',(-0.0878588274613298,0.107979036106918,
0.325498575129534));
#15874=CARTESIAN_POINT('Ctrl Pts',(-0.1383679148179,-0.0152632221501787,
0.33343756476684));
#15875=CARTESIAN_POINT('Ctrl Pts',(-0.0622106591311991,-0.12453304658572,
0.341376554404146));
#15876=CARTESIAN_POINT('Ctrl Pts',(0.0708961914151981,-0.119801401679107,
0.349315544041452));
#15877=CARTESIAN_POINT('Ctrl Pts',(0.1391024375543,-0.00539978406154301,
0.357254533678757));
#15878=CARTESIAN_POINT('Ctrl Pts',(0.0799699354250877,0.113944965792994,
0.365193523316063));
#15879=CARTESIAN_POINT('Ctrl Pts',(-0.0523695618881846,0.128980908622551,
0.373132512953369));
#15880=CARTESIAN_POINT('Ctrl Pts',(-0.136768314413298,0.0259436692471295,
0.381071502590675));
#15881=CARTESIAN_POINT('Ctrl Pts',(-0.0959650484377783,-0.100843221288265,
0.38901049222798));
#15882=CARTESIAN_POINT('Ctrl Pts',(0.0326876424682324,-0.135315053971568,
0.396949481865287));
#15883=CARTESIAN_POINT('Ctrl Pts',(0.13141703692502,-0.0459152284901983,
0.404888471502591));
#15884=CARTESIAN_POINT('Ctrl Pts',(0.109843140674695,0.0855168418978295,
0.412827461139898));
#15885=CARTESIAN_POINT('Ctrl Pts',(-0.0122846228212416,0.13866410438033,
0.420766450777203));
#15886=CARTESIAN_POINT('Ctrl Pts',(-0.123166656044517,0.0648738825743514,
0.428705440414509));
#15887=CARTESIAN_POINT('Ctrl Pts',(-0.121298056821252,-0.0683039326309071,
0.436644430051815));
#15888=CARTESIAN_POINT('Ctrl Pts',(-0.00838939967687663,-0.138954178686792,
0.44458341968912));
#15889=CARTESIAN_POINT('Ctrl Pts',(0.11219917790857,-0.0824013973067221,
0.452522409326426));
#15890=CARTESIAN_POINT('Ctrl Pts',(0.13007709763057,0.0495842159710775,
0.460461398963732));
#15891=CARTESIAN_POINT('Ctrl Pts',(0.0288783492374893,0.136178877755608,
0.468400388601037));
#15892=CARTESIAN_POINT('Ctrl Pts',(-0.0987565487199846,0.0981111099028881,
0.476339378238344));
#15893=CARTESIAN_POINT('Ctrl Pts',(-0.135986594552616,-0.0297706550724338,
0.484278367875649));
#15894=CARTESIAN_POINT('Ctrl Pts',(-0.0487302328423073,-0.130399425645183,
0.492217357512954));
#15895=CARTESIAN_POINT('Ctrl Pts',(0.0831353173341669,-0.111656458896056,
0.50015634715026));
#15896=CARTESIAN_POINT('Ctrl Pts',(0.13889618212661,0.00930034365552528,
0.508095336787567));
#15897=CARTESIAN_POINT('Ctrl Pts',(0.0675071113591811,0.12174331898465,
0.516034326424871));
#15898=CARTESIAN_POINT('Ctrl Pts',(-0.0656800932930844,0.122738629397884,
0.523973316062178));
#15899=CARTESIAN_POINT('Ctrl Pts',(-0.138741673886299,0.0113751364249866,
0.531912305699483));
#15900=CARTESIAN_POINT('Ctrl Pts',(-0.0847947606245053,-0.110401514355972,
0.539851295336789));
#15901=CARTESIAN_POINT('Ctrl Pts',(0.0467759446245483,-0.131113145053959,
0.547790284974095));
#15902=CARTESIAN_POINT('Ctrl Pts',(0.135526478334676,-0.031799677225719,
0.555729274611401));
#15903=CARTESIAN_POINT('Ctrl Pts',(0.100211809365564,0.0966242157284558,
0.563668264248707));
#15904=CARTESIAN_POINT('Ctrl Pts',(-0.0268399031138932,0.136595261273209,
0.571607253886012));
#15905=CARTESIAN_POINT('Ctrl Pts',(-0.129321523751272,0.0515227066069736,
0.579546243523318));
#15906=CARTESIAN_POINT('Ctrl Pts',(-0.113418152377209,-0.0807153548762533,
0.587485233160623));
#15907=CARTESIAN_POINT('Ctrl Pts',(0.00631176444456456,-0.139064040754811,
0.595424222797929));
#15908=CARTESIAN_POINT('Ctrl Pts',(0.120263693490807,-0.0701091280034811,
0.603363212435234));
#15909=CARTESIAN_POINT('Ctrl Pts',(0.124122453355413,0.0630258865426945,
0.611302202072541));
#15910=CARTESIAN_POINT('Ctrl Pts',(0.0143556138404206,0.138465021405133,
0.619241191709845));
#15911=CARTESIAN_POINT('Ctrl Pts',(-0.108552806291007,0.0871489187988374,
0.627180181347153));
#15912=CARTESIAN_POINT('Ctrl Pts',(-0.132088571872698,-0.043946046262323,
0.635119170984457));
#15913=CARTESIAN_POINT('Ctrl Pts',(-0.0347063025259737,-0.134811417789573,
0.643058160621763));
#15914=CARTESIAN_POINT('Ctrl Pts',(0.0944472082050275,-0.102266175560326,
0.65099715025907));
#15915=CARTESIAN_POINT('Ctrl Pts',(0.137140772714236,0.0238967416356601,
0.658936139896373));
#15916=CARTESIAN_POINT('Ctrl Pts',(0.054291358674537,0.128183829614862,
0.666875129533682));
#15917=CARTESIAN_POINT('Ctrl Pts',(-0.0782580734018908,0.115127406593233,
0.674814119170985));
#15918=CARTESIAN_POINT('Ctrl Pts',(-0.139167602654929,-0.00332026696803425,
0.682753108808293));
#15919=CARTESIAN_POINT('Ctrl Pts',(-0.0726787294560835,-0.118728463672822,
0.690692098445597));
#15920=CARTESIAN_POINT('Ctrl Pts',(0.0603425395611779,-0.125448888878168,
0.698631088082904));
#15921=CARTESIAN_POINT('Ctrl Pts',(0.138124349154501,-0.0173294538893964,
0.706570077720209));
#15922=CARTESIAN_POINT('Ctrl Pts',(0.0894627833767505,0.106653908470079,
0.714509067357515));
#15923=CARTESIAN_POINT('Ctrl Pts',(-0.0410958292974484,0.133002927094911,
0.72244805699482));
#15924=CARTESIAN_POINT('Ctrl Pts',(-0.134034026730954,0.0375968812502473,
0.730387046632127));
#15925=CARTESIAN_POINT('Ctrl Pts',(-0.104273258644039,-0.0922265326964679,
0.738326036269432));
#15926=CARTESIAN_POINT('Ctrl Pts',(0.0209425314183671,-0.137622876656644,
0.746265025906738));
#15927=CARTESIAN_POINT('Ctrl Pts',(0.126986869252672,-0.0570349089493802,
0.754204015544043));
#15928=CARTESIAN_POINT('Ctrl Pts',(0.11678343126468,0.0757646090434518,
0.762143005181349));
#15929=CARTESIAN_POINT('Ctrl Pts',(-0.000327234354877375,0.139206819944772,
0.770081994818654));
#15930=CARTESIAN_POINT('Ctrl Pts',(-0.117138339349379,0.0752147276530931,
0.778020984455961));
#15931=CARTESIAN_POINT('Ctrl Pts',(-0.126717322684213,-0.0576312930030564,
0.785959974093266));
#15932=CARTESIAN_POINT('Ctrl Pts',(-0.0202952816069424,-0.137719814645367,
0.793898963730571));
#15933=CARTESIAN_POINT('Ctrl Pts',(0.104705698854998,-0.0917352845351548,
0.801837953367879));
#15934=CARTESIAN_POINT('Ctrl Pts',(0.133855787965376,0.0382266115373486,
0.809776943005182));
#15935=CARTESIAN_POINT('Ctrl Pts',(0.0404700769297216,0.133194664588195,
0.81771593264249));
#15936=CARTESIAN_POINT('Ctrl Pts',(-0.0899632159395838,0.106232130635072,
0.825654922279794));
#15937=CARTESIAN_POINT('Ctrl Pts',(-0.13804135019805,-0.0179786383510676,
0.833593911917101));
#15938=CARTESIAN_POINT('Ctrl Pts',(-0.059752088941783,-0.125731196083361,
0.841532901554406));
#15939=CARTESIAN_POINT('Ctrl Pts',(0.0732361146625898,-0.118385460722959,
0.849471891191712));
#15940=CARTESIAN_POINT('Ctrl Pts',(0.139181674492094,-0.00266594955618734,
0.857410880829018));
#15941=CARTESIAN_POINT('Ctrl Pts',(0.077715950067195,0.115494055719818,
0.865349870466323));
#15942=CARTESIAN_POINT('Ctrl Pts',(-0.0548934004223171,0.127927168308903,
0.87328886010363));
#15943=CARTESIAN_POINT('Ctrl Pts',(-0.137251604915624,0.0232517257326144,
0.881227849740934));
#15944=CARTESIAN_POINT('Ctrl Pts',(-0.0939653715754795,-0.102709078207047,
0.889166839378241));
#15945=CARTESIAN_POINT('Ctrl Pts',(0.0353397195745277,-0.134646760160997,
0.897105829015547));
#15946=CARTESIAN_POINT('Ctrl Pts',(0.132293719443212,-0.0433245611326863,
0.905044818652852));
#15947=CARTESIAN_POINT('Ctrl Pts',(0.108141885842356,0.0876583043865096,
0.912983808290157));
#15948=CARTESIAN_POINT('Ctrl Pts',(-0.0150064327997127,0.138395999855801,
0.920922797927463));
#15949=CARTESIAN_POINT('Ctrl Pts',(-0.124417390671652,0.0624416423544169,
0.928861787564769));
#15950=CARTESIAN_POINT('Ctrl Pts',(-0.119932754264349,-0.0706737593172073,
0.936800777202075));
#15951=CARTESIAN_POINT('Ctrl Pts',(-0.00565790085648466,-0.139092177922979,
0.944739766839381));
#15952=CARTESIAN_POINT('Ctrl Pts',(0.113796373024222,-0.0801812402497705,
0.952678756476687));
#15953=CARTESIAN_POINT('Ctrl Pts',(0.129077866376032,0.0521301276928276,
0.960617746113992));
#15954=CARTESIAN_POINT('Ctrl Pts',(0.026197419344502,0.13671993644362,0.968556735751298));
#15955=CARTESIAN_POINT('Ctrl Pts',(-0.100664969670515,0.0961520134094621,
0.976495725388603));
#15956=CARTESIAN_POINT('Ctrl Pts',(-0.13537547797311,-0.0324364881732178,
0.98443471502591));
#15957=CARTESIAN_POINT('Ctrl Pts',(-0.0461590140787468,-0.131331607851033,
0.992373704663214));
#15958=CARTESIAN_POINT('Ctrl Pts',(0.0853128637208732,-0.110001641284132,
1.00031269430052));
#15959=CARTESIAN_POINT('Ctrl Pts',(0.138686661656432,0.0120272889735618,
1.00825168393783));
#15960=CARTESIAN_POINT('Ctrl Pts',(0.0651023256631918,0.123046060459907,
1.01619067357513));
#15961=CARTESIAN_POINT('Ctrl Pts',(-0.0680787277209358,0.121424596492465,
1.02412966321244));
#15962=CARTESIAN_POINT('Ctrl Pts',(-0.138938371616466,0.00864723620724691,
1.03206865284975));
#15963=CARTESIAN_POINT('Ctrl Pts',(-0.0826094583655966,-0.112046076191904,
1.04000764248705));
#15964=CARTESIAN_POINT('Ctrl Pts',(0.0493427524230464,-0.130168884856471,
1.04794663212436));
#15965=CARTESIAN_POINT('Ctrl Pts',(0.136125055048066,-0.0291310004912345,
1.05588562176166));
#15966=CARTESIAN_POINT('Ctrl Pts',(0.0982941990358779,0.0985743183458784,
1.06382461139897));
#15967=CARTESIAN_POINT('Ctrl Pts',(-0.0295182596522469,0.136041604476578,
1.07176360103627));
#15968=CARTESIAN_POINT('Ctrl Pts',(-0.130308774647192,0.0489721252490281,
1.07970259067358));
#15969=CARTESIAN_POINT('Ctrl Pts',(-0.111810537096203,-0.0829279783650712,
1.08764158031088));
#15970=CARTESIAN_POINT('Ctrl Pts',(0.00904258428980543,-0.13891320121148,
1.09558056994819));
#15971=CARTESIAN_POINT('Ctrl Pts',(0.121617839487272,-0.067732908692211,
1.1035195595855));
#15972=CARTESIAN_POINT('Ctrl Pts',(0.122860297649024,0.0654522196953821,
1.1114585492228));
#15973=CARTESIAN_POINT('Ctrl Pts',(0.0116325734791967,0.138720326685422,
1.11939753886011));
#15974=CARTESIAN_POINT('Ctrl Pts',(-0.110243974478508,0.0849994817198388,
1.12733652849741));
#15975=CARTESIAN_POINT('Ctrl Pts',(-0.131199719314147,-0.0465325633653302,
1.13527551813472));
#15976=CARTESIAN_POINT('Ctrl Pts',(-0.0320511128216771,-0.13546723577438,
1.14321450777202));
#15977=CARTESIAN_POINT('Ctrl Pts',(0.0964380908528195,-0.100390938007982,
1.15115349740933));
#15978=CARTESIAN_POINT('Ctrl Pts',(0.136644831685568,0.0265863832644056,
1.15909248704664));
#15979=CARTESIAN_POINT('Ctrl Pts',(0.0517625939920979,0.129225692742072,
1.16703147668394));
#15980=CARTESIAN_POINT('Ctrl Pts',(-0.0805047509788913,0.113567736929491,
1.17497046632125));
#15981=CARTESIAN_POINT('Ctrl Pts',(-0.139075513779617,-0.00605369873671642,
1.18290945595855));
#15982=CARTESIAN_POINT('Ctrl Pts',(-0.0703321751825429,-0.12013338809653,
1.19084844559586));
#15983=CARTESIAN_POINT('Ctrl Pts',(0.0627954496153871,-0.124239193932754,
1.19878743523316));
#15984=CARTESIAN_POINT('Ctrl Pts',(0.138438143943654,-0.0146125323915816,
1.20672642487047));
#15985=CARTESIAN_POINT('Ctrl Pts',(0.0873502052771435,0.108390901091839,
1.21466541450777));
#15986=CARTESIAN_POINT('Ctrl Pts',(-0.043700859820065,0.132169893139269,
1.22260440414508));
#15987=CARTESIAN_POINT('Ctrl Pts',(-0.134746782767514,0.0349564062120582,
1.23054339378239));
#15988=CARTESIAN_POINT('Ctrl Pts',(-0.102441260891455,-0.0942572748833364,
1.23848238341969));
#15989=CARTESIAN_POINT('Ctrl Pts',(0.0236422145726536,-0.137184880695923,
1.246421373057));
#15990=CARTESIAN_POINT('Ctrl Pts',(0.128082862902196,-0.0545291301253663,
1.2543603626943));
#15991=CARTESIAN_POINT('Ctrl Pts',(0.115272428336817,0.0780443019497631,
1.26229935233161));
#15992=CARTESIAN_POINT('Ctrl Pts',(-0.00306201423577413,0.139173524314926,
1.27023834196891));
#15993=CARTESIAN_POINT('Ctrl Pts',(-0.118593392628464,0.0728989233548558,
1.27817733160622));
#15994=CARTESIAN_POINT('Ctrl Pts',(-0.125560647806918,-0.06010964584811,
1.28611632124353));
#15995=CARTESIAN_POINT('Ctrl Pts',(-0.0175857351491984,-0.138091953858251,
1.29405531088083));
#15996=CARTESIAN_POINT('Ctrl Pts',(0.106487712804436,-0.089660542174548,
1.30199430051814));
#15997=CARTESIAN_POINT('Ctrl Pts',(0.133078957772855,0.0408489510387311,
1.30993329015544));
#15998=CARTESIAN_POINT('Ctrl Pts',(0.0378455373822902,0.133964029124136,
1.31787227979275));
#15999=CARTESIAN_POINT('Ctrl Pts',(-0.0920328787300654,0.104444219726284,
1.32581126943006));
#16000=CARTESIAN_POINT('Ctrl Pts',(-0.137661501842601,-0.0206871148492911,
1.33375025906736));
#16001=CARTESIAN_POINT('Ctrl Pts',(-0.0572704544775333,-0.126880813469472,
1.34168924870467));
#16002=CARTESIAN_POINT('Ctrl Pts',(0.0755477687720905,-0.116923823242002,
1.34962823834197));
#16003=CARTESIAN_POINT('Ctrl Pts',(0.13920718769651,6.89141801743488E-5,
1.35756722797928));
#16004=CARTESIAN_POINT('Ctrl Pts',(0.0754319660950179,0.116998564767658,
1.36550621761658));
#16005=CARTESIAN_POINT('Ctrl Pts',(-0.0573960494825499,0.126824048933643,
1.37344520725389));
#16006=CARTESIAN_POINT('Ctrl Pts',(-0.13768191782304,0.0205508058651932,
1.38138419689119));
#16007=CARTESIAN_POINT('Ctrl Pts',(-0.0919294216917856,-0.104535287252199,
1.3893231865285));
#16008=CARTESIAN_POINT('Ctrl Pts',(0.0379781508110965,-0.133926497290667,
1.39726217616581));
#16009=CARTESIAN_POINT('Ctrl Pts',(0.133119345865688,-0.0407171622080862,
1.40520116580311));
#16010=CARTESIAN_POINT('Ctrl Pts',(0.106398871137127,0.0897659150453452,
1.41314015544042));
#16011=CARTESIAN_POINT('Ctrl Pts',(-0.0177224175491345,0.138074504763813,
1.42107914507772));
#16012=CARTESIAN_POINT('Ctrl Pts',(-0.125620162573399,0.0599852426217579,
1.42901813471503));
#16013=CARTESIAN_POINT('Ctrl Pts',(-0.118521039729242,-0.0730161975746823,
1.43695712435233));
#16014=CARTESIAN_POINT('Ctrl Pts',(-0.00292444232197888,-0.139176693688359,
1.44489611398964));
#16015=CARTESIAN_POINT('Ctrl Pts',(0.115350068603298,-0.0779297424218237,
1.45283510362695));
#16016=CARTESIAN_POINT('Ctrl Pts',(0.128028003046829,0.0546551750765237,
1.46077409326425));
#16017=CARTESIAN_POINT('Ctrl Pts',(0.0235079116789307,0.137209630484779,
1.46871308290156));
#16018=CARTESIAN_POINT('Ctrl Pts',(-0.102537447198224,0.0941531272373115,
1.47665207253886));
#16019=CARTESIAN_POINT('Ctrl Pts',(-0.134706575776555,-0.0350847218495708,
1.48459106217617));
#16020=CARTESIAN_POINT('Ctrl Pts',(-0.0435804807853106,-0.132222740314769,
1.49253005181348));
#16021=CARTESIAN_POINT('Ctrl Pts',(0.0874774386997331,-0.108286040948335,
1.50046904145078));
#16022=CARTESIAN_POINT('Ctrl Pts',(0.138385550162814,0.0147146982980264,
1.50840803108809));
#16023=CARTESIAN_POINT('Ctrl Pts',(0.0627460642121078,0.124368470664037,
1.51634702072539));
#16024=CARTESIAN_POINT('Ctrl Pts',(-0.0706026869052757,0.119928391791904,
1.5242860103627));
#16025=CARTESIAN_POINT('Ctrl Pts',(-0.116004137797729,0.0441355889673283,
1.5295786701209));
#16026=CARTESIAN_POINT('Ctrl Pts',(-0.117668597464313,0.00500517689812487,
1.532225));
#16027=CARTESIAN_POINT('',(0.0684664424539461,-0.0958295198918396,0.));
#16028=CARTESIAN_POINT('Ctrl Pts',(0.0684664424539414,-0.095829519891843,
-1.38777878078145E-17));
#16029=CARTESIAN_POINT('Ctrl Pts',(0.100334321247169,-0.0730611673843044,
0.00264632987910189));
#16030=CARTESIAN_POINT('Ctrl Pts',(0.139021564822767,0.00636891437108143,
0.00793898963730573));
#16031=CARTESIAN_POINT('Ctrl Pts',(0.0699018669780613,0.120491966796142,
0.0158779792746114));
#16032=CARTESIAN_POINT('Ctrl Pts',(-0.0632645460347191,0.123954346655885,
0.0238169689119172));
#16033=CARTESIAN_POINT('Ctrl Pts',(-0.11596266760442,0.0470121293552651,
0.0293787386625077));
#16034=CARTESIAN_POINT('Ctrl Pts',(-0.117944740497024,0.00404481602818191,
0.0322941785339964));
#16035=CARTESIAN_POINT('Ctrl Pts',(-0.117917485785546,7.60014832213644E-5,
0.0325632885263832));
#16036=CARTESIAN_POINT('Ctrl Pts',(0.0635546915223951,0.132092229195826,
-2.16840434497101E-19));
#16037=CARTESIAN_POINT('Ctrl Pts',(0.0668114782730532,0.13015255741457,
-1.00603861447787E-18));
#16038=CARTESIAN_POINT('Ctrl Pts',(0.0699821360194518,0.12808121947321,
-2.9262196004085E-17));
#16039=CARTESIAN_POINT('Ctrl Pts',(0.0730575207853233,0.125877721325919,
-2.71050543121376E-17));
#16040=CARTESIAN_POINT('Ctrl Pts',(0.0789281193465506,0.121671466161783,
-2.36378102375718E-17));
#16041=CARTESIAN_POINT('Ctrl Pts',(0.0844522091809674,0.11698398814956,
1.43782932504085E-18));
#16042=CARTESIAN_POINT('Ctrl Pts',(0.0895990070394484,0.111875963994554,
9.97465998686664E-18));
#16043=CARTESIAN_POINT('Ctrl Pts',(0.0928865546640729,0.108613183302742,
1.54276111490851E-17));
#16044=CARTESIAN_POINT('Ctrl Pts',(0.0960206821069302,0.105176950779614,
-2.53636710091701E-17));
#16045=CARTESIAN_POINT('Ctrl Pts',(0.098978417360439,0.101599719103904,
-1.56125112837913E-17));
#16046=CARTESIAN_POINT('Ctrl Pts',(0.103148772110026,0.0965558852815647,
-1.86354736740503E-18));
#16047=CARTESIAN_POINT('Ctrl Pts',(0.106976174326278,0.0912251680483688,
1.1337629845105E-17));
#16048=CARTESIAN_POINT('Ctrl Pts',(0.110435561611279,0.0856523061447448,
2.03830008427275E-17));
#16049=CARTESIAN_POINT('Ctrl Pts',(0.112407683932559,0.0824753373788608,
2.55395723911076E-17));
#16050=CARTESIAN_POINT('Ctrl Pts',(0.114261188142284,0.0792174064057451,
2.29308760465575E-17));
#16051=CARTESIAN_POINT('Ctrl Pts',(0.115986535786665,0.0758936579718971,
2.08166817117217E-17));
#16052=CARTESIAN_POINT('Ctrl Pts',(0.120573220307724,0.0670577659456877,
1.51962825639422E-17));
#16053=CARTESIAN_POINT('Ctrl Pts',(0.124235263225439,0.0578042025119142,
2.52358375750583E-18));
#16054=CARTESIAN_POINT('Ctrl Pts',(0.126883306113679,0.0482911783993335,
1.30104260698261E-17));
#16055=CARTESIAN_POINT('Ctrl Pts',(0.128478610866444,0.0425600882242624,
1.93281898253259E-17));
#16056=CARTESIAN_POINT('Ctrl Pts',(0.129704960854084,0.0367345196138549,
-5.78096029915021E-19));
#16057=CARTESIAN_POINT('Ctrl Pts',(0.130533291754837,0.0308494671050701,
0.));
#16058=CARTESIAN_POINT('Ctrl Pts',(0.131003715791213,0.0275072397983871,
3.2831114661813E-19));
#16059=CARTESIAN_POINT('Ctrl Pts',(0.131345346899704,0.0241444941465381,
-1.7128612844445E-18));
#16060=CARTESIAN_POINT('Ctrl Pts',(0.131551728167405,0.0207857616715298,
2.60208521396521E-18));
#16061=CARTESIAN_POINT('Ctrl Pts',(0.131851321606701,0.0159100565018035,
8.86587880453295E-18));
#16062=CARTESIAN_POINT('Ctrl Pts',(0.131867617692795,0.0110341713389591,
-1.68111772803455E-17));
#16063=CARTESIAN_POINT('Ctrl Pts',(0.131586936334964,0.0061777758930637,
-6.93889390390723E-18));
#16064=CARTESIAN_POINT('Ctrl Pts',(0.131099036368572,-0.00226395031615145,
9.98510028643051E-18));
#16065=CARTESIAN_POINT('Ctrl Pts',(0.129715139118287,-0.0106479390144509,
1.03491660509995E-17));
#16066=CARTESIAN_POINT('Ctrl Pts',(0.127493709984164,-0.018859987399606,
1.04083408558608E-17));
#16067=CARTESIAN_POINT('Ctrl Pts',(0.126553994220251,-0.0223338732882013,
1.04333731632617E-17));
#16068=CARTESIAN_POINT('Ctrl Pts',(0.125463061762623,-0.0257782540966497,
1.75224609115742E-17));
#16069=CARTESIAN_POINT('Ctrl Pts',(0.124232565886791,-0.0291638780753137,
1.73472347597681E-17));
#16070=CARTESIAN_POINT('Ctrl Pts',(0.12170396813588,-0.0361211392462112,
1.69871551674183E-17));
#16071=CARTESIAN_POINT('Ctrl Pts',(0.118582485980247,-0.0428512226170345,
-6.45748389186585E-19));
#16072=CARTESIAN_POINT('Ctrl Pts',(0.114911168983798,-0.0492778939609075,
3.46944695195361E-18));
#16073=CARTESIAN_POINT('Ctrl Pts',(0.112347970921096,-0.0537647937721124,
6.34254691478841E-18));
#16074=CARTESIAN_POINT('Ctrl Pts',(0.109516356061708,-0.0581036184196785,
-1.05628593522785E-17));
#16075=CARTESIAN_POINT('Ctrl Pts',(0.106427098863261,-0.0622637901458048,
-1.21430643318376E-17));
#16076=CARTESIAN_POINT('Ctrl Pts',(0.104287070791936,-0.0651456752410043,
-1.32377232732828E-17));
#16077=CARTESIAN_POINT('Ctrl Pts',(0.102021590876101,-0.067943056099314,
-1.03088264066386E-17));
#16078=CARTESIAN_POINT('Ctrl Pts',(0.0996491962474235,-0.0706287444932102,
-1.04083408558608E-17));
#16079=CARTESIAN_POINT('Ctrl Pts',(0.0938611946766418,-0.0771810981592459,
-1.06511292104842E-17));
#16080=CARTESIAN_POINT('Ctrl Pts',(0.0874218747326319,-0.0830961188460978,
9.460259835177E-18));
#16081=CARTESIAN_POINT('Ctrl Pts',(0.0803902102994179,-0.0882260767030795,
2.94902990916057E-17));
#16082=CARTESIAN_POINT('Ctrl Pts',(0.0765868618375105,-0.091000813397402,
4.03243227742548E-17));
#16083=CARTESIAN_POINT('Ctrl Pts',(0.0726097989303321,-0.0935451549285004,
-2.49510848448888E-18));
#16084=CARTESIAN_POINT('Ctrl Pts',(0.0684664424539416,-0.0958295198918429,
0.));
#16085=CARTESIAN_POINT('Ctrl Pts',(-0.00156962371674571,0.146072546381438,
1.50365));
#16086=CARTESIAN_POINT('Ctrl Pts',(0.0218361081466035,0.146362061217761,
1.50238307892777));
#16087=CARTESIAN_POINT('Ctrl Pts',(0.0452966847593804,0.141345883428421,
1.50111615785553));
#16088=CARTESIAN_POINT('Ctrl Pts',(0.0660179268768178,0.130913916311315,
1.4998492367833));
#16089=CARTESIAN_POINT('Ctrl Pts',(0.109300214423576,0.109123745727819,
1.4972029069042));
#16090=CARTESIAN_POINT('Ctrl Pts',(0.140630685714559,0.0637042888941242,
1.49455657702509));
#16091=CARTESIAN_POINT('Ctrl Pts',(0.145752650840527,0.0155206226173656,
1.49191024714599));
#16092=CARTESIAN_POINT('Ctrl Pts',(0.150874615966495,-0.0326630436593903,
1.48926391726689));
#16093=CARTESIAN_POINT('Ctrl Pts',(0.129788074927449,-0.0836109193792113,
1.48661758738779));
#16094=CARTESIAN_POINT('Ctrl Pts',(0.0921021927661857,-0.114042242015571,
1.48397125750869));
#16095=CARTESIAN_POINT('Ctrl Pts',(0.0544163106049216,-0.144473564651931,
1.48132492762959));
#16096=CARTESIAN_POINT('Ctrl Pts',(0.000131087321441313,-0.154388334204831,
1.47867859775048));
#16097=CARTESIAN_POINT('Ctrl Pts',(-0.0458840977328367,-0.139228052523514,
1.47603226787138));
#16098=CARTESIAN_POINT('Ctrl Pts',(-0.0918992827871148,-0.124067770842196,
1.47338593799228));
#16099=CARTESIAN_POINT('Ctrl Pts',(-0.129644429612189,-0.0838324379266627,
1.47073960811318));
#16100=CARTESIAN_POINT('Ctrl Pts',(-0.141854649713415,-0.0369491035797489,
1.46809327823408));
#16101=CARTESIAN_POINT('Ctrl Pts',(-0.14497337938942,-0.0249741805295802,
1.46741735368415));
#16102=CARTESIAN_POINT('Ctrl Pts',(-0.146426231435716,-0.0125655473306973,
1.46674142913422));
#16103=CARTESIAN_POINT('Ctrl Pts',(-0.14631473222987,-0.000131398079681141,
1.46606550458429));
#16104=CARTESIAN_POINT('Origin',(0.,0.,-0.0924367114736175));
#16105=CARTESIAN_POINT('',(-0.0684664424539507,-0.0958295198918364,0.));
#16106=CARTESIAN_POINT('Ctrl Pts',(-0.0686146973663072,-0.0959584553529141,
8.16675286424706E-17));
#16107=CARTESIAN_POINT('Ctrl Pts',(-0.0391968190522335,-0.116741470120209,
0.00244290680874874));
#16108=CARTESIAN_POINT('Ctrl Pts',(0.0436301113039178,-0.130476273073809,
0.0075332029917574));
#16109=CARTESIAN_POINT('Ctrl Pts',(0.134092250525203,-0.0374520209666004,
0.0152708885490261));
#16110=CARTESIAN_POINT('Ctrl Pts',(0.104134301645602,0.0924305194826295,
0.023213056671806));
#16111=CARTESIAN_POINT('Ctrl Pts',(-0.0212379681243542,0.137589894578696,
0.0311552247945861));
#16112=CARTESIAN_POINT('Ctrl Pts',(-0.106685947947232,0.0723488109778776,
0.0375631097285225));
#16113=CARTESIAN_POINT('Ctrl Pts',(-0.117663533972591,0.0165813593984342,
0.041323605288199));
#16114=CARTESIAN_POINT('Ctrl Pts',(-0.117600989619072,5.04992496179954E-5,
0.0424367114736154));
#16115=CARTESIAN_POINT('Origin',(0.,0.,0.));
#16116=CARTESIAN_POINT('Ctrl Pts',(-0.0510216505388318,0.106149619882943,
-0.0164977839420939));
#16117=CARTESIAN_POINT('Ctrl Pts',(-0.0863355867949722,0.0891756983861136,
-0.0138503945678339));
#16118=CARTESIAN_POINT('Ctrl Pts',(-0.13808023131828,0.0175094743621551,
-0.00855561581931395));
#16119=CARTESIAN_POINT('Ctrl Pts',(-0.0894531427980795,-0.106808298616542,
-0.000613447696533924));
#16120=CARTESIAN_POINT('Ctrl Pts',(0.0412394829729132,-0.132934609947913,
0.00732872042624606));
#16121=CARTESIAN_POINT('Ctrl Pts',(0.134092250525203,-0.0374520209666004,
0.0152708885490261));
#16122=CARTESIAN_POINT('Ctrl Pts',(0.104134301645602,0.0924305194826295,
0.023213056671806));
#16123=CARTESIAN_POINT('Ctrl Pts',(-0.0212379681243542,0.137589894578696,
0.0311552247945861));
#16124=CARTESIAN_POINT('Ctrl Pts',(-0.127145335141994,0.0567276974868182,
0.039097392917366));
#16125=CARTESIAN_POINT('Ctrl Pts',(-0.116579117211717,-0.0761160149501382,
0.0470395610401461));
#16126=CARTESIAN_POINT('Ctrl Pts',(0.000787973702835166,-0.139222729671589,
0.054981729162926));
#16127=CARTESIAN_POINT('Ctrl Pts',(0.117431922513572,-0.0747907597173192,
0.0629238972857061));
#16128=CARTESIAN_POINT('Ctrl Pts',(0.126496838785129,0.0581591461343325,
0.070866065408486));
#16129=CARTESIAN_POINT('Ctrl Pts',(0.0196773008918215,0.137828289815661,
0.0788082335312661));
#16130=CARTESIAN_POINT('Ctrl Pts',(-0.105168479521776,0.0912330920368172,
0.0867504016540459));
#16131=CARTESIAN_POINT('Ctrl Pts',(-0.133669226619255,-0.0389412707994331,
0.0946925697768262));
#16132=CARTESIAN_POINT('Ctrl Pts',(-0.0397151780004399,-0.133441281507892,
0.102634737899606));
#16133=CARTESIAN_POINT('Ctrl Pts',(0.0906220264938673,-0.105695447092796,
0.110576906022386));
#16134=CARTESIAN_POINT('Ctrl Pts',(0.137940159127448,0.0188783162799928,
0.118519074145166));
#16135=CARTESIAN_POINT('Ctrl Pts',(0.0588909273047484,0.126157580947307,
0.126461242267946));
#16136=CARTESIAN_POINT('Ctrl Pts',(-0.074108440039672,0.117863552156501,
0.134403410390726));
#16137=CARTESIAN_POINT('Ctrl Pts',(-0.139216864956951,0.00159439502933392,
0.142345578513506));
#16138=CARTESIAN_POINT('Ctrl Pts',(-0.0767883381764272,-0.116135388594389,
0.150287746636286));
#16139=CARTESIAN_POINT('Ctrl Pts',(0.0559861945572589,-0.127473226882309,
0.158229914759066));
#16140=CARTESIAN_POINT('Ctrl Pts',(0.137471621702818,-0.0220324926503626,
0.166172082881846));
#16141=CARTESIAN_POINT('Ctrl Pts',(0.0930189202108026,0.103592267873211,
0.174114251004626));
#16142=CARTESIAN_POINT('Ctrl Pts',(-0.0366486683060043,0.134315868829211,
0.182056419127406));
#16143=CARTESIAN_POINT('Ctrl Pts',(-0.132742311638566,0.0419923350165386,
0.189998587250186));
#16144=CARTESIAN_POINT('Ctrl Pts',(-0.107230360350792,-0.0888004916405464,
0.197940755372966));
#16145=CARTESIAN_POINT('Ctrl Pts',(0.0165156171993534,-0.138242945169174,
0.205882923495746));
#16146=CARTESIAN_POINT('Ctrl Pts',(0.125131592687617,-0.061040658666823,
0.213825091618526));
#16147=CARTESIAN_POINT('Ctrl Pts',(0.119114174013628,0.0720811421096423,
0.221767259741306));
#16148=CARTESIAN_POINT('Ctrl Pts',(0.0039759348809324,0.139169211541763,
0.229709427864086));
#16149=CARTESIAN_POINT('Ctrl Pts',(-0.114804669066963,0.0787639858025777,
0.237651595986866));
#16150=CARTESIAN_POINT('Ctrl Pts',(-0.128412401817242,-0.0537971426620367,
0.245593764109646));
#16151=CARTESIAN_POINT('Ctrl Pts',(-0.024381182195918,-0.137074561658528,
0.253535932232426));
#16152=CARTESIAN_POINT('Ctrl Pts',(0.101985705091022,-0.094777599970642,
0.261478100355206));
#16153=CARTESIAN_POINT('Ctrl Pts',(0.134923209124943,0.0343453801629359,
0.269420268477986));
#16154=CARTESIAN_POINT('Ctrl Pts',(0.0442571924125319,0.132004463632409,
0.277362436600766));
#16155=CARTESIAN_POINT('Ctrl Pts',(-0.0869529592639067,0.108733897080731,
0.285304604723546));
#16156=CARTESIAN_POINT('Ctrl Pts',(-0.138505267237684,-0.0141480898545381,
0.293246772846326));
#16157=CARTESIAN_POINT('Ctrl Pts',(-0.0631725212350128,-0.124068972994571,
0.301188940969106));
#16158=CARTESIAN_POINT('Ctrl Pts',(0.0700327441786229,-0.12032993078169,
0.309131109091886));
#16159=CARTESIAN_POINT('Ctrl Pts',(0.139080821187468,-0.00635631000930847,
0.317073277214666));
#16160=CARTESIAN_POINT('Ctrl Pts',(0.0807165776729536,0.11344034374014,
0.325015445337446));
#16161=CARTESIAN_POINT('Ctrl Pts',(-0.0515923433190751,0.129313988454311,
0.332957613460226));
#16162=CARTESIAN_POINT('Ctrl Pts',(-0.136637377548019,0.026722734813544,
0.340899781583006));
#16163=CARTESIAN_POINT('Ctrl Pts',(-0.0965085366518414,-0.100349289247285,
0.348841949705786));
#16164=CARTESIAN_POINT('Ctrl Pts',(0.0320320385160992,-0.135491055083419,
0.356784117828566));
#16165=CARTESIAN_POINT('Ctrl Pts',(0.131227975626944,-0.0465090949381858,
0.364726285951346));
#16166=CARTESIAN_POINT('Ctrl Pts',(0.110205605501345,0.0850799742312894,
0.372668454074126));
#16167=CARTESIAN_POINT('Ctrl Pts',(-0.0117764211155082,0.138727046407055,
0.380610622196906));
#16168=CARTESIAN_POINT('Ctrl Pts',(-0.122970036152848,0.065285892102983,
0.388552790319686));
#16169=CARTESIAN_POINT('Ctrl Pts',(-0.121510464882371,-0.0679638464419502,
0.396494958442466));
#16170=CARTESIAN_POINT('Ctrl Pts',(-0.00873482453528946,-0.138951719454826,
0.404437126565246));
#16171=CARTESIAN_POINT('Ctrl Pts',(0.112042812448737,-0.0826455423945668,
0.412379294688026));
#16172=CARTESIAN_POINT('Ctrl Pts',(0.130177722634257,0.049372441998279,
0.420321462810806));
#16173=CARTESIAN_POINT('Ctrl Pts',(0.0290564652212241,0.136160197297018,
0.428263630933586));
#16174=CARTESIAN_POINT('Ctrl Pts',(-0.098683499418539,0.098211223603141,
0.436205799056366));
#16175=CARTESIAN_POINT('Ctrl Pts',(-0.136019240449831,-0.0297093205335648,
0.444147967179146));
#16176=CARTESIAN_POINT('Ctrl Pts',(-0.0487473834415776,-0.130413074907061,
0.452090135301926));
#16177=CARTESIAN_POINT('Ctrl Pts',(0.0831820848081396,-0.111645054821459,
0.460032303424706));
#16178=CARTESIAN_POINT('Ctrl Pts',(0.138908217753341,0.00940130521287039,
0.467974471547486));
#16179=CARTESIAN_POINT('Ctrl Pts',(0.0673801526530663,0.121835103839429,
0.475916639670265));
#16180=CARTESIAN_POINT('Ctrl Pts',(-0.0658750545035054,0.12265543075329,
0.483858807793047));
#16181=CARTESIAN_POINT('Ctrl Pts',(-0.138781944133385,0.0111107822259715,
0.491800975915825));
#16182=CARTESIAN_POINT('Ctrl Pts',(-0.084550315326251,-0.110612484274364,
0.499743144038607));
#16183=CARTESIAN_POINT('Ctrl Pts',(0.0471380885036503,-0.131003351527116,
0.507685312161385));
#16184=CARTESIAN_POINT('Ctrl Pts',(0.135643160584381,-0.031381690295376,
0.515627480284167));
#16185=CARTESIAN_POINT('Ctrl Pts',(0.0998851624184703,0.0969888232104648,
0.523569648406945));
#16186=CARTESIAN_POINT('Ctrl Pts',(-0.0273779061153799,0.136507610615132,
0.531511816529727));
#16187=CARTESIAN_POINT('Ctrl Pts',(-0.129560000008381,0.0509714027366644,
0.539453984652505));
#16188=CARTESIAN_POINT('Ctrl Pts',(-0.113051823689188,-0.0812598465397498,
0.547396152775286));
#16189=CARTESIAN_POINT('Ctrl Pts',(0.00702343738442799,-0.139048728244533,
0.555338320898066));
#16190=CARTESIAN_POINT('Ctrl Pts',(0.12066450826877,-0.0694546898587181,
0.563280489020846));
#16191=CARTESIAN_POINT('Ctrl Pts',(0.123764493242992,0.063766979789076,
0.571222657143626));
#16192=CARTESIAN_POINT('Ctrl Pts',(0.0134834875971477,0.13857154491934,
0.579164825266405));
#16193=CARTESIAN_POINT('Ctrl Pts',(-0.109149777898995,0.0864303389077871,
0.587106993389186));
#16194=CARTESIAN_POINT('Ctrl Pts',(-0.131790633456927,-0.0448899368693808,
0.595049161511966));
#16195=CARTESIAN_POINT('Ctrl Pts',(-0.0336977294021144,-0.135086418755761,
0.602991329634746));
#16196=CARTESIAN_POINT('Ctrl Pts',(0.0952657566843092,-0.101529863106778,
0.610933497757526));
#16197=CARTESIAN_POINT('Ctrl Pts',(0.136956022624868,0.025038477707157,
0.618875665880307));
#16198=CARTESIAN_POINT('Ctrl Pts',(0.0531805018142573,0.128669000640787,
0.626817834003085));
#16199=CARTESIAN_POINT('Ctrl Pts',(-0.0793138220987445,0.114425500318782,
0.634760002125867));
#16200=CARTESIAN_POINT('Ctrl Pts',(-0.139148536750765,-0.00464351367351466,
0.642702170248646));
#16201=CARTESIAN_POINT('Ctrl Pts',(-0.0715088964667609,-0.119458592094588,
0.650644338371427));
#16202=CARTESIAN_POINT('Ctrl Pts',(0.0616402393688536,-0.124837327709565,
0.658586506494205));
#16203=CARTESIAN_POINT('Ctrl Pts',(0.138320583400205,-0.0158522461166236,
0.666528674616987));
#16204=CARTESIAN_POINT('Ctrl Pts',(0.0882850628235238,0.107655121482266,
0.674470842739765));
#16205=CARTESIAN_POINT('Ctrl Pts',(-0.0426286451686149,0.132539337972556,
0.682413010862546));
#16206=CARTESIAN_POINT('Ctrl Pts',(-0.13449013477919,0.0360039045964495,
0.690355178985326));
#16207=CARTESIAN_POINT('Ctrl Pts',(-0.103144844235522,-0.0935148042116587,
0.698297347108106));
#16208=CARTESIAN_POINT('Ctrl Pts',(0.022691720100341,-0.137364345221032,
0.706239515230886));
#16209=CARTESIAN_POINT('Ctrl Pts',(0.127740337615313,-0.0553740340325759,
0.714181683353665));
#16210=CARTESIAN_POINT('Ctrl Pts',(0.115765682611161,0.077344581120379,
0.722123851476446));
#16211=CARTESIAN_POINT('Ctrl Pts',(-0.00226223072526165,0.139207614056346,
0.730066019599226));
#16212=CARTESIAN_POINT('Ctrl Pts',(-0.118217708309552,0.0735421711751344,
0.738008187722006));
#16213=CARTESIAN_POINT('Ctrl Pts',(-0.125873620115675,-0.059495455776806,
0.745950355844786));
#16214=CARTESIAN_POINT('Ctrl Pts',(-0.0182163644075178,-0.138029133036789,
0.753892523967566));
#16215=CARTESIAN_POINT('Ctrl Pts',(0.106128952536144,-0.0901139441634624,
0.761834692090347));
#16216=CARTESIAN_POINT('Ctrl Pts',(0.133249245915149,0.0403548753208232,
0.769776860213125));
#16217=CARTESIAN_POINT('Ctrl Pts',(0.0382995408207276,0.133854483197375,
0.777719028335907));
#16218=CARTESIAN_POINT('Ctrl Pts',(-0.0917364783268051,0.104729633071593,
0.785661196458685));
#16219=CARTESIAN_POINT('Ctrl Pts',(-0.137732458880487,-0.0203383202317681,
0.793603364581467));
#16220=CARTESIAN_POINT('Ctrl Pts',(-0.0575513573065257,-0.126774282767806,
0.801545532704245));
#16221=CARTESIAN_POINT('Ctrl Pts',(0.0753527000357912,-0.117071978271622,
0.809487700827026));
#16222=CARTESIAN_POINT('Ctrl Pts',(0.139225942868322,-0.000119714417332432,
0.817429868949805));
#16223=CARTESIAN_POINT('Ctrl Pts',(0.0755539188089132,0.116942220141962,
0.825372037072586));
#16224=CARTESIAN_POINT('Ctrl Pts',(-0.0573332568284509,0.12687306712048,
0.833314205195366));
#16225=CARTESIAN_POINT('Ctrl Pts',(-0.13769727914169,0.0205751504512258,
0.841256373318145));
#16226=CARTESIAN_POINT('Ctrl Pts',(-0.0919164475821765,-0.104571717796869,
0.849198541440926));
#16227=CARTESIAN_POINT('Ctrl Pts',(0.0380692928980519,-0.133920149482284,
0.857140709563706));
#16228=CARTESIAN_POINT('Ctrl Pts',(0.133179650076608,-0.0405839661022353,
0.865082877686486));
#16229=CARTESIAN_POINT('Ctrl Pts',(0.106283765719693,0.0899312995767124,
0.873025045809266));
#16230=CARTESIAN_POINT('Ctrl Pts',(-0.0179789669825735,0.138060255849953,
0.880967213932046));
#16231=CARTESIAN_POINT('Ctrl Pts',(-0.125771118879347,0.0597118342956578,
0.888909382054826));
#16232=CARTESIAN_POINT('Ctrl Pts',(-0.118344004924669,-0.0733387619032726,
0.896851550177606));
#16233=CARTESIAN_POINT('Ctrl Pts',(-0.00250162451743248,-0.139203517821528,
0.904793718300386));
#16234=CARTESIAN_POINT('Ctrl Pts',(0.115632500949424,-0.0775435504945224,
0.912735886423165));
#16235=CARTESIAN_POINT('Ctrl Pts',(0.127835376168433,0.0551542754370876,
0.920678054545947));
#16236=CARTESIAN_POINT('Ctrl Pts',(0.0229279137899797,0.137325118854324,
0.928620222668725));
#16237=CARTESIAN_POINT('Ctrl Pts',(-0.102983873094174,0.0936920454555137,
0.936562390791507));
#16238=CARTESIAN_POINT('Ctrl Pts',(-0.134551852288801,-0.0357725669300891,
0.944504558914285));
#16239=CARTESIAN_POINT('Ctrl Pts',(-0.0428565117498991,-0.132465832952297,
0.952446727037066));
#16240=CARTESIAN_POINT('Ctrl Pts',(0.0880997963686447,-0.107806787258123,
0.960388895159846));
#16241=CARTESIAN_POINT('Ctrl Pts',(0.138347640177547,0.0156143509765511,
0.968331063282625));
#16242=CARTESIAN_POINT('Ctrl Pts',(0.061854832590724,0.124731139593481,
0.976273231405407));
#16243=CARTESIAN_POINT('Ctrl Pts',(-0.0713033562375951,0.119581390225944,
0.984215399528185));
#16244=CARTESIAN_POINT('Ctrl Pts',(-0.139140345480169,0.00488280234845834,
0.992157567650966));
#16245=CARTESIAN_POINT('Ctrl Pts',(-0.0795104838321055,-0.114288934109561,
1.00009973577375));
#16246=CARTESIAN_POINT('Ctrl Pts',(0.0529591494285269,-0.128760265574912,
1.00804190389653));
#16247=CARTESIAN_POINT('Ctrl Pts',(0.136912761112491,-0.0252739657289669,
1.0159840720193));
#16248=CARTESIAN_POINT('Ctrl Pts',(0.0954402180350474,0.101365883217864,
1.02392624014209));
#16249=CARTESIAN_POINT('Ctrl Pts',(-0.0334653697086341,0.135144169424284,
1.03186840826486));
#16250=CARTESIAN_POINT('Ctrl Pts',(-0.131713240771149,0.0451165125500212,
1.03981057638765));
#16251=CARTESIAN_POINT('Ctrl Pts',(-0.109298251871946,-0.0862425048155002,
1.04775274451043));
#16252=CARTESIAN_POINT('Ctrl Pts',(0.0132451643780021,-0.13859452774087,
1.05569491263321));
#16253=CARTESIAN_POINT('Ctrl Pts',(0.123654649330263,-0.0639797248987874,
1.06363708075599));
#16254=CARTESIAN_POINT('Ctrl Pts',(0.120783771971213,0.0692470788374567,
1.07157924887876));
#16255=CARTESIAN_POINT('Ctrl Pts',(0.00726255089817806,0.139036444335888,
1.07952141700155));
#16256=CARTESIAN_POINT('Ctrl Pts',(-0.112911912907791,0.0814541430660127,
1.08746358512433));
#16257=CARTESIAN_POINT('Ctrl Pts',(-0.129647464608677,-0.0507485213543897,
1.09540575324711));
#16258=CARTESIAN_POINT('Ctrl Pts',(-0.0276126195379174,-0.136460326620484,
1.10334792136989));
#16259=CARTESIAN_POINT('Ctrl Pts',(0.0997182217817603,-0.0971604536002107,
1.11129008949267));
#16260=CARTESIAN_POINT('Ctrl Pts',(0.135696927507188,0.0311483765905046,
1.11923225761545));
#16261=CARTESIAN_POINT('Ctrl Pts',(0.0473633069609982,0.130922093830007,
1.12717442573822));
#16262=CARTESIAN_POINT('Ctrl Pts',(-0.0843599685788644,0.110757722983492,
1.13511659386101));
#16263=CARTESIAN_POINT('Ctrl Pts',(-0.138800846271631,-0.0108721006891078,
1.14305876198379));
#16264=CARTESIAN_POINT('Ctrl Pts',(-0.0660858892268601,-0.122541963197144,
1.15100093010657));
#16265=CARTESIAN_POINT('Ctrl Pts',(0.0671705316110708,-0.121950798202395,
1.15894309822935));
#16266=CARTESIAN_POINT('Ctrl Pts',(0.138891844802359,-0.00964017357273747,
1.16688526635212));
#16267=CARTESIAN_POINT('Ctrl Pts',(0.0833739592533277,0.111501840422208,
1.17482743447491));
#16268=CARTESIAN_POINT('Ctrl Pts',(-0.0485230383040216,0.130496713571114,
1.18276960259768));
#16269=CARTESIAN_POINT('Ctrl Pts',(-0.135967947813762,0.0299431906521225,
1.19071177072047));
#16270=CARTESIAN_POINT('Ctrl Pts',(-0.0988522486080867,-0.0980413710850678,
1.19865393884324));
#16271=CARTESIAN_POINT('Ctrl Pts',(0.0288222657999454,-0.136209964735594,
1.20659610696603));
#16272=CARTESIAN_POINT('Ctrl Pts',(0.130092623711363,-0.0495962373069701,
1.21453827508881));
#16273=CARTESIAN_POINT('Ctrl Pts',(0.112184773380136,0.082452738709893,
1.22248044321158));
#16274=CARTESIAN_POINT('Ctrl Pts',(-0.00849585454694533,0.138966535376798,
1.23042261133437));
#16275=CARTESIAN_POINT('Ctrl Pts',(-0.121393406896754,0.0681727090639588,
1.23836477945715));
#16276=CARTESIAN_POINT('Ctrl Pts',(-0.123082127310551,-0.0650743223999996,
1.24630694757992));
#16277=CARTESIAN_POINT('Ctrl Pts',(-0.0120149744006178,-0.138706589206355,
1.25424911570271));
#16278=CARTESIAN_POINT('Ctrl Pts',(0.110059129405696,-0.0852693704304675,
1.26219128382548));
#16279=CARTESIAN_POINT('Ctrl Pts',(0.13130776387206,0.0462833517151888,
1.27013345194827));
#16280=CARTESIAN_POINT('Ctrl Pts',(0.0322649968732001,0.135435768819968,
1.27807562007105));
#16281=CARTESIAN_POINT('Ctrl Pts',(-0.0963358219719167,0.100515107841202,
1.28601778819382));
#16282=CARTESIAN_POINT('Ctrl Pts',(-0.136683130933199,-0.0264877182308561,
1.29395995631661));
#16283=CARTESIAN_POINT('Ctrl Pts',(-0.0518146499729274,-0.129225073214149,
1.30190212443939));
#16284=CARTESIAN_POINT('Ctrl Pts',(0.0805213734929343,-0.11357898534207,
1.30984429256217));
#16285=CARTESIAN_POINT('Ctrl Pts',(0.1390915465469,0.0061171215252809,1.31778646068495));
#16286=CARTESIAN_POINT('Ctrl Pts',(0.0702395735793815,0.120209316621791,
1.32572862880773));
#16287=CARTESIAN_POINT('Ctrl Pts',(-0.0629590648350173,0.124177428154433,
1.33367079693051));
#16288=CARTESIAN_POINT('Ctrl Pts',(-0.138480731711197,0.0143862582011507,
1.34161296505328));
#16289=CARTESIAN_POINT('Ctrl Pts',(-0.0871398218994898,-0.108584202098263,
1.34955513317607));
#16290=CARTESIAN_POINT('Ctrl Pts',(0.0440301174146577,-0.132080378229483,
1.35749730129884));
#16291=CARTESIAN_POINT('Ctrl Pts',(0.13486394497766,-0.0345773583278084,
1.36543946942163));
#16292=CARTESIAN_POINT('Ctrl Pts',(0.102148545386143,0.0946020732301706,
1.3733816375444));
#16293=CARTESIAN_POINT('Ctrl Pts',(-0.0241454188302812,0.137116288461919,
1.38132380566719));
#16294=CARTESIAN_POINT('Ctrl Pts',(-0.128319693277533,0.0540178939468163,
1.38926597378996));
#16295=CARTESIAN_POINT('Ctrl Pts',(-0.114939956470138,-0.0785664351508689,
1.39720814191275));
#16296=CARTESIAN_POINT('Ctrl Pts',(0.00373660876362508,-0.139175849115243,
1.40515031003553));
#16297=CARTESIAN_POINT('Ctrl Pts',(0.118990018389619,-0.0722858665142316,
1.41309247815831));
#16298=CARTESIAN_POINT('Ctrl Pts',(0.125236419206141,0.0608253567263532,
1.42103464628109));
#16299=CARTESIAN_POINT('Ctrl Pts',(0.0167532566496359,0.13821437898841,
1.42897681440387));
#16300=CARTESIAN_POINT('Ctrl Pts',(-0.107077349343502,0.0889846891406984,
1.43691898252665));
#16301=CARTESIAN_POINT('Ctrl Pts',(-0.132814597987359,-0.0417638487589672,
1.44486115064943));
#16302=CARTESIAN_POINT('Ctrl Pts',(-0.0368790902657646,-0.134252921254984,
1.45280331877221));
#16303=CARTESIAN_POINT('Ctrl Pts',(0.0928396680879532,-0.103751556080299,
1.46074548689499));
#16304=CARTESIAN_POINT('Ctrl Pts',(0.137511141307062,0.0217950526079239,
1.46868765501776));
#16305=CARTESIAN_POINT('Ctrl Pts',(0.0562018483347667,0.127378648737854,
1.47662982314055));
#16306=CARTESIAN_POINT('Ctrl Pts',(-0.0765818961642769,0.116263681173923,
1.48457199126332));
#16307=CARTESIAN_POINT('Ctrl Pts',(-0.13923195096087,-0.00134816270381636,
1.49251415938611));
#16308=CARTESIAN_POINT('Ctrl Pts',(-0.0742871760264013,-0.117748889605885,
1.50045632750888));
#16309=CARTESIAN_POINT('Ctrl Pts',(0.0586284551779338,-0.126233948370975,
1.50839849563167));
#16310=CARTESIAN_POINT('Ctrl Pts',(0.137995068118234,-0.019163470063063,
1.51634066375444));
#16311=CARTESIAN_POINT('Ctrl Pts',(0.0906261803825392,0.105639137646141,
1.52428283187723));
#16312=CARTESIAN_POINT('Ctrl Pts',(0.00417072711528833,0.124051375507138,
1.52957761062575));
#16313=CARTESIAN_POINT('Ctrl Pts',(-0.0334019664627544,0.1129391839063,
1.53222500000001));
#16314=CARTESIAN_POINT('Ctrl Pts',(-0.0551480035117261,0.114734422509858,
-0.0109985226280628));
#16315=CARTESIAN_POINT('Ctrl Pts',(-0.093317938433455,0.0963877427684319,
-0.00835113325380276));
#16316=CARTESIAN_POINT('Ctrl Pts',(-0.149247407742026,0.0189255452031589,
-0.00305635450528277));
#16317=CARTESIAN_POINT('Ctrl Pts',(-0.0966876253720675,-0.115446371588928,
0.00488581361749726));
#16318=CARTESIAN_POINT('Ctrl Pts',(0.0445747075563756,-0.143685636564375,
0.0128279817402772));
#16319=CARTESIAN_POINT('Ctrl Pts',(0.144936900801175,-0.0404809362687151,
0.0207701498630572));
#16320=CARTESIAN_POINT('Ctrl Pts',(0.112556116319125,0.0999057960529736,
0.0287123179858373));
#16321=CARTESIAN_POINT('Ctrl Pts',(-0.0229555792165621,0.148717415239805,
0.0366544861086172));
#16322=CARTESIAN_POINT('Ctrl Pts',(-0.137428156769908,0.0613155244327884,
0.0445966542313972));
#16323=CARTESIAN_POINT('Ctrl Pts',(-0.126007400730642,-0.0822718633254329,
0.0525388223541772));
#16324=CARTESIAN_POINT('Ctrl Pts',(0.000851700720621877,-0.150482305134309,
0.0604809904769572));
#16325=CARTESIAN_POINT('Ctrl Pts',(0.126929176276611,-0.0808394286734405,
0.0684231585997372));
#16326=CARTESIAN_POINT('Ctrl Pts',(0.136727213562698,0.0628627408439891,
0.0763653267225173));
#16327=CARTESIAN_POINT('Ctrl Pts',(0.0212686937255662,0.148975090584026,
0.0843074948452972));
#16328=CARTESIAN_POINT('Ctrl Pts',(-0.113673932864549,0.0986115272026031,
0.0922496629680772));
#16329=CARTESIAN_POINT('Ctrl Pts',(-0.144479665027646,-0.0420906285100245,
0.100191831090857));
#16330=CARTESIAN_POINT('Ctrl Pts',(-0.0429271251068198,-0.144233284958223,
0.108133999213637));
#16331=CARTESIAN_POINT('Ctrl Pts',(0.0979510420095061,-0.114243518700172,
0.116076167336417));
#16332=CARTESIAN_POINT('Ctrl Pts',(0.149096007275942,0.0204050915936607,
0.124018335459197));
#16333=CARTESIAN_POINT('Ctrl Pts',(0.0636537044864716,0.136360518400275,
0.131960503581977));
#16334=CARTESIAN_POINT('Ctrl Pts',(-0.0801019266996435,0.127395713772213,
0.139902671704757));
#16335=CARTESIAN_POINT('Ctrl Pts',(-0.15047596611352,0.00172334100814176,
0.147844839827537));
#16336=CARTESIAN_POINT('Ctrl Pts',(-0.0829985603893774,-0.125527785761544,
0.155787007950317));
#16337=CARTESIAN_POINT('Ctrl Pts',(0.0605140527882773,-0.137782566606816,
0.163729176073097));
#16338=CARTESIAN_POINT('Ctrl Pts',(0.148589577098441,-0.0238143605552183,
0.171671344195877));
#16339=CARTESIAN_POINT('Ctrl Pts',(0.100541783424623,0.111970245809892,
0.179613512318657));
#16340=CARTESIAN_POINT('Ctrl Pts',(-0.0396126128240685,0.145178604134651,
0.187555680441437));
#16341=CARTESIAN_POINT('Ctrl Pts',(-0.143477786216001,0.0453884461694337,
0.195497848564217));
#16342=CARTESIAN_POINT('Ctrl Pts',(-0.115902567375552,-0.095982191346566,
0.203440016686997));
#16343=CARTESIAN_POINT('Ctrl Pts',(0.0178513102906219,-0.149423281002214,
0.211382184809777));
#16344=CARTESIAN_POINT('Ctrl Pts',(0.135251553802876,-0.0659772944027704,
0.219324352932557));
#16345=CARTESIAN_POINT('Ctrl Pts',(0.128747479107914,0.07791067196398,0.227266521055337));
#16346=CARTESIAN_POINT('Ctrl Pts',(0.00429748682099232,0.150424458749874,
0.235208689178117));
#16347=CARTESIAN_POINT('Ctrl Pts',(-0.124089444892588,0.0851339876261335,
0.243150857300897));
#16348=CARTESIAN_POINT('Ctrl Pts',(-0.138797696890977,-0.0581479623084488,
0.251093025423677));
#16349=CARTESIAN_POINT('Ctrl Pts',(-0.0263529993083425,-0.148160405002171,
0.259035193546457));
#16350=CARTESIAN_POINT('Ctrl Pts',(0.110233752987369,-0.102442695616748,
0.266977361669237));
#16351=CARTESIAN_POINT('Ctrl Pts',(0.145835062802846,0.0371230472913779,
0.274919529792017));
#16352=CARTESIAN_POINT('Ctrl Pts',(0.0478364728857143,0.142680265085169,
0.282861697914797));
#16353=CARTESIAN_POINT('Ctrl Pts',(-0.0939852406223356,0.117527701960322,
0.290803866037577));
#16354=CARTESIAN_POINT('Ctrl Pts',(-0.14970681824969,-0.01529231023972,
0.298746034160357));
#16355=CARTESIAN_POINT('Ctrl Pts',(-0.0682815703945392,-0.134102995221473,
0.306688202283137));
#16356=CARTESIAN_POINT('Ctrl Pts',(0.0756966107742644,-0.1300615596562,
0.314630370405917));
#16357=CARTESIAN_POINT('Ctrl Pts',(0.150328919865546,-0.00687037371415525,
0.322572538528697));
#16358=CARTESIAN_POINT('Ctrl Pts',(0.0872444944832666,0.122614780370367,
0.330514706651477));
#16359=CARTESIAN_POINT('Ctrl Pts',(-0.0557648508131485,0.139772198940638,
0.338456874774257));
#16360=CARTESIAN_POINT('Ctrl Pts',(-0.147687863823926,0.0288839239377102,
0.346399042897038));
#16361=CARTESIAN_POINT('Ctrl Pts',(-0.104313621021262,-0.10846499275041,
0.354341211019817));
#16362=CARTESIAN_POINT('Ctrl Pts',(0.0346226151823369,-0.146448833047075,
0.362283379142597));
#16363=CARTESIAN_POINT('Ctrl Pts',(0.141840978962514,-0.0502704970123603,
0.370225547265377));
#16364=CARTESIAN_POINT('Ctrl Pts',(0.119118434135606,0.0919607787700563,
0.378167715388157));
#16365=CARTESIAN_POINT('Ctrl Pts',(-0.0127288338612142,0.149946533709345,
0.386109883510937));
#16366=CARTESIAN_POINT('Ctrl Pts',(-0.132915182358376,0.070565859178174,
0.394052051633717));
#16367=CARTESIAN_POINT('Ctrl Pts',(-0.131337568919768,-0.0734603918663599,
0.401994219756497));
#16368=CARTESIAN_POINT('Ctrl Pts',(-0.00944124952954395,-0.150189377088511,
0.409936387879277));
#16369=CARTESIAN_POINT('Ctrl Pts',(0.121104224366159,-0.0893294633566384,
0.417878556002057));
#16370=CARTESIAN_POINT('Ctrl Pts',(0.140705787232781,0.0533654159743681,
0.425820724124838));
#16371=CARTESIAN_POINT('Ctrl Pts',(0.0314063937394313,0.147172091835368,
0.433762892247617));
#16372=CARTESIAN_POINT('Ctrl Pts',(-0.106664482920656,0.106154012011714,
0.441705060370398));
#16373=CARTESIAN_POINT('Ctrl Pts',(-0.147019735166745,-0.032112048430678,
0.449647228493177));
#16374=CARTESIAN_POINT('Ctrl Pts',(-0.052689806088835,-0.14096017351449,
0.457589396615958));
#16375=CARTESIAN_POINT('Ctrl Pts',(0.0899093983958942,-0.120674298270189,
0.465531564738737));
#16376=CARTESIAN_POINT('Ctrl Pts',(0.15014235720654,0.0101616315312987,
0.473473732861518));
#16377=CARTESIAN_POINT('Ctrl Pts',(0.0728294921055832,0.131688462906045,
0.481415900984297));
#16378=CARTESIAN_POINT('Ctrl Pts',(-0.071202669822089,0.132575133389036,
0.489358069107078));
#16379=CARTESIAN_POINT('Ctrl Pts',(-0.150005871264529,0.012009361726732,
0.497300237229857));
#16380=CARTESIAN_POINT('Ctrl Pts',(-0.0913882839399832,-0.119558219045865,
0.505242405352637));
#16381=CARTESIAN_POINT('Ctrl Pts',(0.0509503601487159,-0.141598188489932,
0.513184573475417));
#16382=CARTESIAN_POINT('Ctrl Pts',(0.146613240011817,-0.0339196703426114,
0.521126741598197));
#16383=CARTESIAN_POINT('Ctrl Pts',(0.107963329873666,0.104832750538675,
0.529068909720978));
#16384=CARTESIAN_POINT('Ctrl Pts',(-0.0295920819230583,0.147547602048875,
0.537011077843756));
#16385=CARTESIAN_POINT('Ctrl Pts',(-0.140038106568177,0.055093691941219,
0.544953245966537));
#16386=CARTESIAN_POINT('Ctrl Pts',(-0.122194838935542,-0.0878316999746162,
0.552895414089317));
#16387=CARTESIAN_POINT('Ctrl Pts',(0.00759145471482065,-0.150294231420327,
0.560837582212097));
#16388=CARTESIAN_POINT('Ctrl Pts',(0.130423195946632,-0.0750718065719766,
0.568779750334878));
#16389=CARTESIAN_POINT('Ctrl Pts',(0.133773890807325,0.0689241055160235,
0.576721918457657));
#16390=CARTESIAN_POINT('Ctrl Pts',(0.0145739585745413,0.149778456108953,
0.584664086580438));
#16391=CARTESIAN_POINT('Ctrl Pts',(-0.117977216952174,0.0934203535806499,
0.592606254703216));
#16392=CARTESIAN_POINT('Ctrl Pts',(-0.142449141490696,-0.0485203902651028,
0.600548422825998));
#16393=CARTESIAN_POINT('Ctrl Pts',(-0.036423018067407,-0.146011471938939,
0.608490590948776));
#16394=CARTESIAN_POINT('Ctrl Pts',(0.102970331784443,-0.109741044988262,
0.616432759071558));
#16395=CARTESIAN_POINT('Ctrl Pts',(0.148032279177632,0.0270634532975707,
0.624374927194337));
#16396=CARTESIAN_POINT('Ctrl Pts',(0.0574814509102497,0.139075048028633,
0.632317095317117));
#16397=CARTESIAN_POINT('Ctrl Pts',(-0.0857282916847416,0.123679611042927,
0.640259263439898));
#16398=CARTESIAN_POINT('Ctrl Pts',(-0.150402111894479,-0.00501905574730406,
0.648201431562677));
#16399=CARTESIAN_POINT('Ctrl Pts',(-0.0772921462128499,-0.129119751845818,
0.656143599685457));
#16400=CARTESIAN_POINT('Ctrl Pts',(0.0666253659236285,-0.134933490277457,
0.664085767808237));
#16401=CARTESIAN_POINT('Ctrl Pts',(0.14950719819016,-0.0171342893707992,
0.672027935931017));
#16402=CARTESIAN_POINT('Ctrl Pts',(0.0954250774564579,0.11636168087194,
0.679970104053797));
#16403=CARTESIAN_POINT('Ctrl Pts',(-0.0460762176180427,0.143258397146306,
0.687912272176577));
#16404=CARTESIAN_POINT('Ctrl Pts',(-0.145366963764729,0.0389157041403328,
0.695854440299358));
#16405=CARTESIAN_POINT('Ctrl Pts',(-0.111486636987321,-0.101077771820372,
0.703796608422136));
#16406=CARTESIAN_POINT('Ctrl Pts',(0.02452690272786,-0.148473624679578,
0.711738776544918));
#16407=CARTESIAN_POINT('Ctrl Pts',(0.138071279799868,-0.0598523840572839,
0.719680944667696));
#16408=CARTESIAN_POINT('Ctrl Pts',(0.125128179973684,0.0835997892305201,
0.727623112790477));
#16409=CARTESIAN_POINT('Ctrl Pts',(-0.00244518761474098,0.150465967050502,
0.735565280913257));
#16410=CARTESIAN_POINT('Ctrl Pts',(-0.127778512144395,0.0794898610961098,
0.743507449036036));
#16411=CARTESIAN_POINT('Ctrl Pts',(-0.136053592364468,-0.0643071239260258,
0.751449617158818));
#16412=CARTESIAN_POINT('Ctrl Pts',(-0.019689604662082,-0.149192176910068,
0.759391785281597));
#16413=CARTESIAN_POINT('Ctrl Pts',(0.114712083700712,-0.0974018687498071,
0.767333953404378));
#16414=CARTESIAN_POINT('Ctrl Pts',(0.144025718573537,0.0436185576594447,
0.775276121527157));
#16415=CARTESIAN_POINT('Ctrl Pts',(0.0413969989087525,0.14467990414796,
0.783218289649938));
#16416=CARTESIAN_POINT('Ctrl Pts',(-0.0991556246317344,0.113199594905656,
0.791160457772717));
#16417=CARTESIAN_POINT('Ctrl Pts',(-0.148871509365196,-0.021983172706469,
0.799102625895497));
#16418=CARTESIAN_POINT('Ctrl Pts',(-0.062205797368885,-0.137027095702329,
0.807044794018277));
#16419=CARTESIAN_POINT('Ctrl Pts',(0.081446815661698,-0.126540121706451,
0.814986962141057));
#16420=CARTESIAN_POINT('Ctrl Pts',(0.150485778196879,-0.000129396266831759,
0.822929130263837));
#16421=CARTESIAN_POINT('Ctrl Pts',(0.0816643079123276,0.126399869446589,
0.830871298386618));
#16422=CARTESIAN_POINT('Ctrl Pts',(-0.0619700581130299,0.137133869194964,
0.838813466509397));
#16423=CARTESIAN_POINT('Ctrl Pts',(-0.148833484480893,0.0222391564630926,
0.846755634632177));
#16424=CARTESIAN_POINT('Ctrl Pts',(-0.0993501488194509,-0.113028908304323,
0.854697802754957));
#16425=CARTESIAN_POINT('Ctrl Pts',(0.041148129789194,-0.144750881164039,
0.862639970877736));
#16426=CARTESIAN_POINT('Ctrl Pts',(0.143950494202948,-0.0438661760544617,
0.870582139000517));
#16427=CARTESIAN_POINT('Ctrl Pts',(0.114879417330645,0.0972044528644933,
0.878524307123298));
#16428=CARTESIAN_POINT('Ctrl Pts',(-0.0194330078274841,0.149225816766708,
0.886466475246077));
#16429=CARTESIAN_POINT('Ctrl Pts',(-0.135942801386891,0.0645410019599824,
0.894408643368857));
#16430=CARTESIAN_POINT('Ctrl Pts',(-0.127915022941288,-0.0792700011911429,
0.902350811491637));
#16431=CARTESIAN_POINT('Ctrl Pts',(-0.00270394227186439,-0.150461539534541,
0.910292979614417));
#16432=CARTESIAN_POINT('Ctrl Pts',(0.124984227305131,-0.0838148501630433,
0.918235147737197));
#16433=CARTESIAN_POINT('Ctrl Pts',(0.138174004553101,0.0596148525845174,
0.926177315859977));
#16434=CARTESIAN_POINT('Ctrl Pts',(0.0247821984756025,0.148431225898158,
0.934119483982757));
#16435=CARTESIAN_POINT('Ctrl Pts',(-0.11131264737753,0.101269347369872,
0.942061652105537));
#16436=CARTESIAN_POINT('Ctrl Pts',(-0.145433672650089,-0.0386656571445607,
0.950003820228317));
#16437=CARTESIAN_POINT('Ctrl Pts',(-0.0463225128062989,-0.143178947440692,
0.957945988351097));
#16438=CARTESIAN_POINT('Ctrl Pts',(0.0952248276606132,-0.116525612549003,
0.965888156473877));
#16439=CARTESIAN_POINT('Ctrl Pts',(0.149536443172165,0.0168771545685866,
0.973830324596656));
#16440=CARTESIAN_POINT('Ctrl Pts',(0.0668573142755158,0.134818714245386,
0.981772492719438));
#16441=CARTESIAN_POINT('Ctrl Pts',(-0.0770699830103684,0.129252481220654,
0.989714660842216));
#16442=CARTESIAN_POINT('Ctrl Pts',(-0.15039325815857,0.00527769678589187,
0.997656828964997));
#16443=CARTESIAN_POINT('Ctrl Pts',(-0.0859408583470751,-0.123532000103139,
1.00559899708778));
#16444=CARTESIAN_POINT('Ctrl Pts',(0.0572421967501742,-0.139173693973137,
1.01354116521056));
#16445=CARTESIAN_POINT('Ctrl Pts',(0.147985518909957,-0.0273179863069172,
1.02148333333334));
#16446=CARTESIAN_POINT('Ctrl Pts',(0.103158902618224,0.109563803299803,
1.02942550145612));
#16447=CARTESIAN_POINT('Ctrl Pts',(-0.0361718663885326,0.146073893166727,
1.0373676695789));
#16448=CARTESIAN_POINT('Ctrl Pts',(-0.142365489706367,0.0487652901517079,
1.04530983770168));
#16449=CARTESIAN_POINT('Ctrl Pts',(-0.118137698690712,-0.0932173284908804,
1.05325200582446));
#16450=CARTESIAN_POINT('Ctrl Pts',(0.0143163610725534,-0.149803297655807,
1.06119417394724));
#16451=CARTESIAN_POINT('Ctrl Pts',(0.133655163317704,-0.0691540562905145,
1.06913634207002));
#16452=CARTESIAN_POINT('Ctrl Pts',(0.130552105047211,0.0748474051030229,
1.0770785101928));
#16453=CARTESIAN_POINT('Ctrl Pts',(0.0078499064261323,0.150280954056111,
1.08502067831558));
#16454=CARTESIAN_POINT('Ctrl Pts',(-0.122043612932812,0.0880417101447944,
1.09296284643836));
#16455=CARTESIAN_POINT('Ctrl Pts',(-0.140132644828567,-0.0548527851276936,
1.10090501456114));
#16456=CARTESIAN_POINT('Ctrl Pts',(-0.0298457776877653,-0.147496493982489,
1.10884718268392));
#16457=CARTESIAN_POINT('Ctrl Pts',(0.107782887988268,-0.10501826145877,
1.1167893508067));
#16458=CARTESIAN_POINT('Ctrl Pts',(0.146671355310253,0.033667487497105,
1.12473151892948));
#16459=CARTESIAN_POINT('Ctrl Pts',(0.0511937930472066,0.141510359113225,
1.13267368705226));
#16460=CARTESIAN_POINT('Ctrl Pts',(-0.0911825429852659,0.119715203870077,
1.14061585517504));
#16461=CARTESIAN_POINT('Ctrl Pts',(-0.150026302104679,-0.0117513769282424,
1.14855802329782));
#16462=CARTESIAN_POINT('Ctrl Pts',(-0.0714305557085884,-0.132452489195471,
1.1565001914206));
#16463=CARTESIAN_POINT('Ctrl Pts',(0.0726029180563751,-0.131813513998426,
1.16444235954338));
#16464=CARTESIAN_POINT('Ctrl Pts',(0.150124660100533,-0.010419818262018,
1.17238452766616));
#16465=CARTESIAN_POINT('Ctrl Pts',(0.0901167906002831,0.120519501471002,
1.18032669578894));
#16466=CARTESIAN_POINT('Ctrl Pts',(-0.0524473171394798,0.141050576417769,
1.18826886391172));
#16467=CARTESIAN_POINT('Ctrl Pts',(-0.146964294261872,0.0323648326895764,
1.1962110320345));
#16468=CARTESIAN_POINT('Ctrl Pts',(-0.106846879624786,-0.105970422747861,
1.20415320015727));
#16469=CARTESIAN_POINT('Ctrl Pts',(0.0311532535456026,-0.14722588419309,
1.21209536828006));
#16470=CARTESIAN_POINT('Ctrl Pts',(0.140613805972886,-0.0536073106276968,
1.22003753640283));
#16471=CARTESIAN_POINT('Ctrl Pts',(0.121257666323848,0.0891210667609394,
1.22797970452562));
#16472=CARTESIAN_POINT('Ctrl Pts',(-0.00918295295119051,0.150205391241489,
1.2359218726484));
#16473=CARTESIAN_POINT('Ctrl Pts',(-0.131211043922368,0.0736861461587066,
1.24386404077118));
#16474=CARTESIAN_POINT('Ctrl Pts',(-0.133036338837895,-0.0703371788708997,
1.25180620889396));
#16475=CARTESIAN_POINT('Ctrl Pts',(-0.0129866800356469,-0.149924422041766,
1.25974837701674));
#16476=CARTESIAN_POINT('Ctrl Pts',(0.118960111851797,-0.0921654923014072,
1.26769054513952));
#16477=CARTESIAN_POINT('Ctrl Pts',(0.141927220045961,0.050026496908035,
1.2756327132623));
#16478=CARTESIAN_POINT('Ctrl Pts',(0.0348744139414821,0.146389075532006,
1.28357488138508));
#16479=CARTESIAN_POINT('Ctrl Pts',(-0.104126938119509,0.108644221848311,
1.29151704950786));
#16480=CARTESIAN_POINT('Ctrl Pts',(-0.147737317493493,-0.0286299004949125,
1.29945921763064));
#16481=CARTESIAN_POINT('Ctrl Pts',(-0.0560051364173496,-0.139676092720537,
1.30740138575342));
#16482=CARTESIAN_POINT('Ctrl Pts',(0.0870335032532438,-0.122764634549313,
1.3153435538762));
#16483=CARTESIAN_POINT('Ctrl Pts',(0.150340512633584,0.00661184096937889,
1.32328572199898));
#16484=CARTESIAN_POINT('Ctrl Pts',(0.0759201674095095,0.129931190880528,
1.33122789012176));
#16485=CARTESIAN_POINT('Ctrl Pts',(-0.0680508508044829,0.134220221643466,
1.33917005824454));
#16486=CARTESIAN_POINT('Ctrl Pts',(-0.149680298423566,0.0155497403439283,
1.34711222636732));
#16487=CARTESIAN_POINT('Ctrl Pts',(-0.0941872156892785,-0.117365900463673,
1.3550543944901));
#16488=CARTESIAN_POINT('Ctrl Pts',(0.0475910332998192,-0.142762319241037,
1.36299656261288));
#16489=CARTESIAN_POINT('Ctrl Pts',(0.145771005694385,-0.0373737865856905,
1.37093873073566));
#16490=CARTESIAN_POINT('Ctrl Pts',(0.110409762917901,0.10225297323032,1.37888089885844));
#16491=CARTESIAN_POINT('Ctrl Pts',(-0.0260981686868614,0.148205506441964,
1.38682306698121));
#16492=CARTESIAN_POINT('Ctrl Pts',(-0.138697490589939,0.0583865667538053,
1.394765235104));
#16493=CARTESIAN_POINT('Ctrl Pts',(-0.124235673603468,-0.0849204601545819,
1.40270740322677));
#16494=CARTESIAN_POINT('Ctrl Pts',(0.0040388053119065,-0.150431633134115,
1.41064957134956));
#16495=CARTESIAN_POINT('Ctrl Pts',(0.12861328245382,-0.0781319533624403,
1.41859173947234));
#16496=CARTESIAN_POINT('Ctrl Pts',(0.1353648581188,0.0657445800149866,1.42653390759512));
#16497=CARTESIAN_POINT('Ctrl Pts',(0.0181081687242482,0.149392404544468,
1.43447607571789));
#16498=CARTESIAN_POINT('Ctrl Pts',(-0.115737181672069,0.0961812857364522,
1.44241824384068));
#16499=CARTESIAN_POINT('Ctrl Pts',(-0.143555918690644,-0.0451414811888502,
1.45036041196346));
#16500=CARTESIAN_POINT('Ctrl Pts',(-0.0398616700558823,-0.145110565703753,
1.45830258008624));
#16501=CARTESIAN_POINT('Ctrl Pts',(0.100348034367198,-0.112142416378873,
1.46624474820902));
#16502=CARTESIAN_POINT('Ctrl Pts',(0.14863229283285,0.0235577176564554,
1.4741869163318));
#16503=CARTESIAN_POINT('Ctrl Pts',(0.0607471474677608,0.137680339497592,
1.48212908445458));
#16504=CARTESIAN_POINT('Ctrl Pts',(-0.0827754224726193,0.125666453945577,
1.49007125257736));
#16505=CARTESIAN_POINT('Ctrl Pts',(-0.150492272191201,-0.00145719475437189,
1.49801342070014));
#16506=CARTESIAN_POINT('Ctrl Pts',(-0.0802951178786721,-0.12727177793954,
1.50595558882292));
#16507=CARTESIAN_POINT('Ctrl Pts',(0.0633700050447994,-0.136443062004882,
1.5138977569457));
#16508=CARTESIAN_POINT('Ctrl Pts',(0.149155357006591,-0.0207133070603065,
1.52183992506848));
#16509=CARTESIAN_POINT('Ctrl Pts',(0.0979555318420461,0.114182655252422,
1.52978209319126));
#16510=CARTESIAN_POINT('Ctrl Pts',(0.00450803278943675,0.134083974545181,
1.53507687193978));
#16511=CARTESIAN_POINT('Ctrl Pts',(-0.0361033354337414,0.122073089461022,
1.53772426131404));
#16512=CARTESIAN_POINT('Ctrl Pts',(-0.0592743564846203,0.123319225136773,
-0.00549926131403157));
#16513=CARTESIAN_POINT('Ctrl Pts',(-0.100300290071938,0.10359978715075,
-0.00285187193977157));
#16514=CARTESIAN_POINT('Ctrl Pts',(-0.160414584165772,0.0203416160441626,
0.00244290680874841));
#16515=CARTESIAN_POINT('Ctrl Pts',(-0.103922107946056,-0.124084444561314,
0.0103850749315284));
#16516=CARTESIAN_POINT('Ctrl Pts',(0.0479099321398382,-0.154436663180837,
0.0183272430543084));
#16517=CARTESIAN_POINT('Ctrl Pts',(0.155781551077148,-0.0435098515708298,
0.0262694111770884));
#16518=CARTESIAN_POINT('Ctrl Pts',(0.120977930992648,0.107381072623318,
0.0342115792998684));
#16519=CARTESIAN_POINT('Ctrl Pts',(-0.0246731903087699,0.159844935900913,
0.0421537474226484));
#16520=CARTESIAN_POINT('Ctrl Pts',(-0.147710978397823,0.0659033513787588,
0.0500959155454284));
#16521=CARTESIAN_POINT('Ctrl Pts',(-0.135435684249567,-0.0884277117007276,
0.0580380836682085));
#16522=CARTESIAN_POINT('Ctrl Pts',(0.000915427738408385,-0.16174188059703,
0.0659802517909884));
#16523=CARTESIAN_POINT('Ctrl Pts',(0.13642643003965,-0.0868880976295618,
0.0739224199137684));
#16524=CARTESIAN_POINT('Ctrl Pts',(0.146957588340267,0.0675663355536457,
0.0818645880365484));
#16525=CARTESIAN_POINT('Ctrl Pts',(0.0228600865593111,0.160121891352391,
0.0898067561593285));
#16526=CARTESIAN_POINT('Ctrl Pts',(-0.122179386207322,0.105989962368389,
0.0977489242821083));
#16527=CARTESIAN_POINT('Ctrl Pts',(-0.155290103436038,-0.0452399862206161,
0.105691092404888));
#16528=CARTESIAN_POINT('Ctrl Pts',(-0.0461390722131997,-0.155025288408554,
0.113633260527668));
#16529=CARTESIAN_POINT('Ctrl Pts',(0.105280057525145,-0.122791590307548,
0.121575428650448));
#16530=CARTESIAN_POINT('Ctrl Pts',(0.160251855424436,0.0219318669073289,
0.129517596773229));
#16531=CARTESIAN_POINT('Ctrl Pts',(0.0684164816681947,0.146563455853242,
0.137459764896008));
#16532=CARTESIAN_POINT('Ctrl Pts',(-0.086095413359615,0.136927875387926,
0.145401933018789));
#16533=CARTESIAN_POINT('Ctrl Pts',(-0.16173506727009,0.00185228698694943,
0.153344101141568));
#16534=CARTESIAN_POINT('Ctrl Pts',(-0.0892087826023274,-0.134920182928699,
0.161286269264348));
#16535=CARTESIAN_POINT('Ctrl Pts',(0.0650419110192955,-0.148091906331324,
0.169228437387128));
#16536=CARTESIAN_POINT('Ctrl Pts',(0.159707532494063,-0.025596228460074,
0.177170605509908));
#16537=CARTESIAN_POINT('Ctrl Pts',(0.108064646638443,0.120348223746572,
0.185112773632688));
#16538=CARTESIAN_POINT('Ctrl Pts',(-0.0425765573421325,0.156041339440091,
0.193054941755468));
#16539=CARTESIAN_POINT('Ctrl Pts',(-0.154213260793436,0.0487845573223287,
0.200997109878248));
#16540=CARTESIAN_POINT('Ctrl Pts',(-0.124574774400312,-0.103163891052585,
0.208939278001028));
#16541=CARTESIAN_POINT('Ctrl Pts',(0.0191870033818907,-0.160603616835255,
0.216881446123808));
#16542=CARTESIAN_POINT('Ctrl Pts',(0.145371514918136,-0.0709139301387177,
0.224823614246588));
#16543=CARTESIAN_POINT('Ctrl Pts',(0.138380784202201,0.0837402018183176,
0.232765782369368));
#16544=CARTESIAN_POINT('Ctrl Pts',(0.00461903876105218,0.161679705957985,
0.240707950492149));
#16545=CARTESIAN_POINT('Ctrl Pts',(-0.133374220718213,0.0915039894496894,
0.248650118614928));
#16546=CARTESIAN_POINT('Ctrl Pts',(-0.149182991964712,-0.0624987819548612,
0.256592286737709));
#16547=CARTESIAN_POINT('Ctrl Pts',(-0.0283248164207669,-0.159246248345813,
0.264534454860488));
#16548=CARTESIAN_POINT('Ctrl Pts',(0.118481800883715,-0.110107791262854,
0.272476622983269));
#16549=CARTESIAN_POINT('Ctrl Pts',(0.156746916480749,0.0399007144198201,
0.280418791106048));
#16550=CARTESIAN_POINT('Ctrl Pts',(0.0514157533588968,0.153356066537929,
0.288360959228829));
#16551=CARTESIAN_POINT('Ctrl Pts',(-0.101017521980764,0.126321506839912,
0.296303127351608));
#16552=CARTESIAN_POINT('Ctrl Pts',(-0.160908369261695,-0.0164365306249019,
0.304245295474388));
#16553=CARTESIAN_POINT('Ctrl Pts',(-0.0733906195540655,-0.144137017448375,
0.312187463597168));
#16554=CARTESIAN_POINT('Ctrl Pts',(0.0813604773699057,-0.13979318853071,
0.320129631719948));
#16555=CARTESIAN_POINT('Ctrl Pts',(0.161577018543625,-0.00738443741900211,
0.328071799842729));
#16556=CARTESIAN_POINT('Ctrl Pts',(0.0937724112935796,0.131789217000595,
0.336013967965508));
#16557=CARTESIAN_POINT('Ctrl Pts',(-0.0599373583072218,0.150230409426965,
0.343956136088289));
#16558=CARTESIAN_POINT('Ctrl Pts',(-0.158738350099833,0.0310451130618767,
0.351898304211068));
#16559=CARTESIAN_POINT('Ctrl Pts',(-0.112118705390683,-0.116580696253536,
0.359840472333849));
#16560=CARTESIAN_POINT('Ctrl Pts',(0.0372131918485748,-0.15740661101073,
0.367782640456628));
#16561=CARTESIAN_POINT('Ctrl Pts',(0.152453982298084,-0.0540318990865351,
0.375724808579408));
#16562=CARTESIAN_POINT('Ctrl Pts',(0.128031262769868,0.0988415833088236,
0.383666976702188));
#16563=CARTESIAN_POINT('Ctrl Pts',(-0.0136812466069205,0.161166021011634,
0.391609144824968));
#16564=CARTESIAN_POINT('Ctrl Pts',(-0.142860328563903,0.0758458262533652,
0.399551312947749));
#16565=CARTESIAN_POINT('Ctrl Pts',(-0.141164672957165,-0.0789569372907697,
0.407493481070528));
#16566=CARTESIAN_POINT('Ctrl Pts',(-0.0101476745237983,-0.161427034722196,
0.415435649193308));
#16567=CARTESIAN_POINT('Ctrl Pts',(0.130165636283581,-0.0960133843187101,
0.423377817316089));
#16568=CARTESIAN_POINT('Ctrl Pts',(0.151233851831306,0.0573583899504574,
0.431319985438868));
#16569=CARTESIAN_POINT('Ctrl Pts',(0.0337563222576384,0.158183986373718,
0.439262153561649));
#16570=CARTESIAN_POINT('Ctrl Pts',(-0.114645466422773,0.114096800420287,
0.447204321684428));
#16571=CARTESIAN_POINT('Ctrl Pts',(-0.158020229883659,-0.0345147763277912,
0.455146489807208));
#16572=CARTESIAN_POINT('Ctrl Pts',(-0.0566322287360923,-0.151507272121918,
0.463088657929988));
#16573=CARTESIAN_POINT('Ctrl Pts',(0.0966367119836487,-0.129703541718919,
0.471030826052768));
#16574=CARTESIAN_POINT('Ctrl Pts',(0.161376496659739,0.0109219578497271,
0.478972994175549));
#16575=CARTESIAN_POINT('Ctrl Pts',(0.0782788315581001,0.141541821972661,
0.486915162298328));
#16576=CARTESIAN_POINT('Ctrl Pts',(-0.0765302851406724,0.142494836024782,
0.494857330421108));
#16577=CARTESIAN_POINT('Ctrl Pts',(-0.161229798395673,0.0129079412274925,
0.502799498543889));
#16578=CARTESIAN_POINT('Ctrl Pts',(-0.0982262525537151,-0.128503953817366,
0.510741666666668));
#16579=CARTESIAN_POINT('Ctrl Pts',(0.0547626317937811,-0.152193025452748,
0.518683834789449));
#16580=CARTESIAN_POINT('Ctrl Pts',(0.157583319439253,-0.0364576503898468,
0.526626002912228));
#16581=CARTESIAN_POINT('Ctrl Pts',(0.116041497328862,0.112676677866884,
0.534568171035008));
#16582=CARTESIAN_POINT('Ctrl Pts',(-0.0318062577307366,0.158587593482618,
0.542510339157789));
#16583=CARTESIAN_POINT('Ctrl Pts',(-0.150516213127973,0.0592159811457737,
0.550452507280567));
#16584=CARTESIAN_POINT('Ctrl Pts',(-0.131337854181896,-0.0944035534094825,
0.558394675403349));
#16585=CARTESIAN_POINT('Ctrl Pts',(0.00815947204521347,-0.161539734596121,
0.566336843526128));
#16586=CARTESIAN_POINT('Ctrl Pts',(0.140181883624494,-0.080688923285235,
0.574279011648909));
#16587=CARTESIAN_POINT('Ctrl Pts',(0.143783288371658,0.0740812312429708,
0.582221179771688));
#16588=CARTESIAN_POINT('Ctrl Pts',(0.0156644295519346,0.160985367298567,
0.590163347894469));
#16589=CARTESIAN_POINT('Ctrl Pts',(-0.126804656005353,0.100410368253513,
0.598105516017247));
#16590=CARTESIAN_POINT('Ctrl Pts',(-0.153107649524464,-0.0521508436608248,
0.606047684140029));
#16591=CARTESIAN_POINT('Ctrl Pts',(-0.0391483067326994,-0.156936525122116,
0.613989852262808));
#16592=CARTESIAN_POINT('Ctrl Pts',(0.110674906884577,-0.117952226869747,
0.621932020385589));
#16593=CARTESIAN_POINT('Ctrl Pts',(0.159108535730396,0.0290884288879846,
0.629874188508368));
#16594=CARTESIAN_POINT('Ctrl Pts',(0.061782400006242,0.14948109541648,0.637816356631148));
#16595=CARTESIAN_POINT('Ctrl Pts',(-0.0921427612707386,0.132933721767072,
0.645758524753929));
#16596=CARTESIAN_POINT('Ctrl Pts',(-0.161655687038194,-0.0053945978210935,
0.653700692876707));
#16597=CARTESIAN_POINT('Ctrl Pts',(-0.0830753959589387,-0.138780911597048,
0.661642860999489));
#16598=CARTESIAN_POINT('Ctrl Pts',(0.0716104924784035,-0.145029652845349,
0.669585029122267));
#16599=CARTESIAN_POINT('Ctrl Pts',(0.160693812980115,-0.0184163326249747,
0.677527197245049));
#16600=CARTESIAN_POINT('Ctrl Pts',(0.102565092089392,0.125068240261613,
0.685469365367828));
#16601=CARTESIAN_POINT('Ctrl Pts',(-0.0495237900674707,0.153977456320057,
0.693411533490608));
#16602=CARTESIAN_POINT('Ctrl Pts',(-0.156243792750268,0.0418275036842162,
0.701353701613389));
#16603=CARTESIAN_POINT('Ctrl Pts',(-0.119828429739121,-0.108640739429086,
0.709295869736167));
#16604=CARTESIAN_POINT('Ctrl Pts',(0.0263620853553792,-0.159582904138124,
0.717238037858949));
#16605=CARTESIAN_POINT('Ctrl Pts',(0.148402221984423,-0.0643307340819919,
0.725180205981728));
#16606=CARTESIAN_POINT('Ctrl Pts',(0.134490677336207,0.0898549973406614,
0.733122374104509));
#16607=CARTESIAN_POINT('Ctrl Pts',(-0.00262814450422035,0.161724320044658,
0.741064542227287));
#16608=CARTESIAN_POINT('Ctrl Pts',(-0.137339315979238,0.0854375510170853,
0.749006710350069));
#16609=CARTESIAN_POINT('Ctrl Pts',(-0.146233564613262,-0.0691187920752458,
0.756948878472847));
#16610=CARTESIAN_POINT('Ctrl Pts',(-0.0211628449166461,-0.160355220783347,
0.764891046595629));
#16611=CARTESIAN_POINT('Ctrl Pts',(0.12329521486528,-0.104689793336152,
0.772833214718408));
#16612=CARTESIAN_POINT('Ctrl Pts',(0.154802191231926,0.0468822399980663,
0.780775382841188));
#16613=CARTESIAN_POINT('Ctrl Pts',(0.0444944569967772,0.155505325098544,
0.788717550963968));
#16614=CARTESIAN_POINT('Ctrl Pts',(-0.106574770936664,0.121669556739719,
0.796659719086747));
#16615=CARTESIAN_POINT('Ctrl Pts',(-0.160010559849905,-0.0236280251811701,
0.804601887209529));
#16616=CARTESIAN_POINT('Ctrl Pts',(-0.0668602374312443,-0.147279908636853,
0.812544055332307));
#16617=CARTESIAN_POINT('Ctrl Pts',(0.0875409312876049,-0.13600826514128,
0.820486223455089));
#16618=CARTESIAN_POINT('Ctrl Pts',(0.161745613525436,-0.000139078116330951,
0.828428391577867));
#16619=CARTESIAN_POINT('Ctrl Pts',(0.0877746970157421,0.135857518751215,
0.836370559700649));
#16620=CARTESIAN_POINT('Ctrl Pts',(-0.0666068593976089,0.147394671269449,
0.844312727823428));
#16621=CARTESIAN_POINT('Ctrl Pts',(-0.159969689820096,0.0239031624749592,
0.852254895946208));
#16622=CARTESIAN_POINT('Ctrl Pts',(-0.106783850056725,-0.121486098811777,
0.860197064068988));
#16623=CARTESIAN_POINT('Ctrl Pts',(0.0442269666803361,-0.155581612845794,
0.868139232191768));
#16624=CARTESIAN_POINT('Ctrl Pts',(0.154721338329289,-0.0471483860066884,
0.876081400314548));
#16625=CARTESIAN_POINT('Ctrl Pts',(0.123475068941597,0.104477606152275,
0.884023568437328));
#16626=CARTESIAN_POINT('Ctrl Pts',(-0.0208870486723946,0.160391377683462,
0.891965736560109));
#16627=CARTESIAN_POINT('Ctrl Pts',(-0.146114483894434,0.0693701696243073,
0.899907904682887));
#16628=CARTESIAN_POINT('Ctrl Pts',(-0.137486040957907,-0.0852012404790134,
0.907850072805669));
#16629=CARTESIAN_POINT('Ctrl Pts',(-0.00290626002629624,-0.161719561247554,
0.915792240928448));
#16630=CARTESIAN_POINT('Ctrl Pts',(0.134335953660838,-0.0900861498315643,
0.923734409051229));
#16631=CARTESIAN_POINT('Ctrl Pts',(0.148512632937768,0.0640754297319473,
0.931676577174007));
#16632=CARTESIAN_POINT('Ctrl Pts',(0.0266364831612253,0.159537332941991,
0.939618745296788));
#16633=CARTESIAN_POINT('Ctrl Pts',(-0.119641421660886,0.10884664928423,
0.947560913419568));
#16634=CARTESIAN_POINT('Ctrl Pts',(-0.156315493011378,-0.0415587473590326,
0.955503081542348));
#16635=CARTESIAN_POINT('Ctrl Pts',(-0.0497885138626987,-0.153892061929087,
0.963445249665127));
#16636=CARTESIAN_POINT('Ctrl Pts',(0.102349858952582,-0.125244437839883,
0.971387417787908));
#16637=CARTESIAN_POINT('Ctrl Pts',(0.160725246166783,0.018139958160622,
0.979329585910688));
#16638=CARTESIAN_POINT('Ctrl Pts',(0.0718597959603077,0.14490628889729,
0.987271754033468));
#16639=CARTESIAN_POINT('Ctrl Pts',(-0.0828366097831417,0.138923572215364,
0.995213922156248));
#16640=CARTESIAN_POINT('Ctrl Pts',(-0.161646170836971,0.00567259122332548,
1.00315609027903));
#16641=CARTESIAN_POINT('Ctrl Pts',(-0.0923712328620446,-0.132775066096718,
1.01109825840181));
#16642=CARTESIAN_POINT('Ctrl Pts',(0.0615252440718216,-0.149587122371362,
1.01904042652459));
#16643=CARTESIAN_POINT('Ctrl Pts',(0.159058276707423,-0.0293620068848675,
1.02698259464737));
#16644=CARTESIAN_POINT('Ctrl Pts',(0.1108775872014,0.117761723381742,1.03492476277015));
#16645=CARTESIAN_POINT('Ctrl Pts',(-0.0388783630684312,0.157003616909169,
1.04286693089293));
#16646=CARTESIAN_POINT('Ctrl Pts',(-0.153017738641585,0.0524140677533946,
1.05080909901571));
#16647=CARTESIAN_POINT('Ctrl Pts',(-0.126977145509477,-0.10019215216626,
1.05875126713849));
#16648=CARTESIAN_POINT('Ctrl Pts',(0.0153875577671049,-0.161012067570745,
1.06669343526127));
#16649=CARTESIAN_POINT('Ctrl Pts',(0.143655677305146,-0.0743283876822416,
1.07463560338405));
#16650=CARTESIAN_POINT('Ctrl Pts',(0.140320438123209,0.080447731368589,
1.08257777150683));
#16651=CARTESIAN_POINT('Ctrl Pts',(0.00843726195408678,0.161525463776335,
1.09051993962961));
#16652=CARTESIAN_POINT('Ctrl Pts',(-0.131175312957834,0.094629277223576,
1.09846210775239));
#16653=CARTESIAN_POINT('Ctrl Pts',(-0.150617825048456,-0.0589570489009974,
1.10640427587517));
#16654=CARTESIAN_POINT('Ctrl Pts',(-0.0320789358376135,-0.158532661344495,
1.11434644399795));
#16655=CARTESIAN_POINT('Ctrl Pts',(0.115847554194776,-0.112876069317329,
1.12228861212073));
#16656=CARTESIAN_POINT('Ctrl Pts',(0.157645783113317,0.0361865984037055,
1.13023078024351));
#16657=CARTESIAN_POINT('Ctrl Pts',(0.0550242791334153,0.152098624396442,
1.13817294836629));
#16658=CARTESIAN_POINT('Ctrl Pts',(-0.0980051173916675,0.128672684756662,
1.14611511648907));
#16659=CARTESIAN_POINT('Ctrl Pts',(-0.161251757937727,-0.0126306531673768,
1.15405728461185));
#16660=CARTESIAN_POINT('Ctrl Pts',(-0.0767752221903169,-0.142363015193798,
1.16199945273463));
#16661=CARTESIAN_POINT('Ctrl Pts',(0.0780353045016797,-0.141676229794458,
1.16994162085741));
#16662=CARTESIAN_POINT('Ctrl Pts',(0.161357475398708,-0.0111994629512984,
1.17788378898019));
#16663=CARTESIAN_POINT('Ctrl Pts',(0.0968596219472387,0.129537162519796,
1.18582595710297));
#16664=CARTESIAN_POINT('Ctrl Pts',(-0.0563715959749383,0.151604439264423,
1.19376812522575));
#16665=CARTESIAN_POINT('Ctrl Pts',(-0.157960640709981,0.0347864747270306,
1.20171029334853));
#16666=CARTESIAN_POINT('Ctrl Pts',(-0.114841510641486,-0.113899474410655,
1.20965246147131));
#16667=CARTESIAN_POINT('Ctrl Pts',(0.03348424129126,-0.158241803650584,
1.21759462959409));
#16668=CARTESIAN_POINT('Ctrl Pts',(0.151134988234409,-0.0576183839484237,
1.22553679771687));
#16669=CARTESIAN_POINT('Ctrl Pts',(0.130330559267559,0.0957893948119858,
1.23347896583965));
#16670=CARTESIAN_POINT('Ctrl Pts',(-0.0098700513554357,0.16144424710618,
1.24142113396243));
#16671=CARTESIAN_POINT('Ctrl Pts',(-0.141028680947982,0.0791995832534545,
1.24936330208521));
#16672=CARTESIAN_POINT('Ctrl Pts',(-0.142990550365238,-0.0756000353418,
1.25730547020799));
#16673=CARTESIAN_POINT('Ctrl Pts',(-0.013958385670676,-0.161142254877177,
1.26524763833077));
#16674=CARTESIAN_POINT('Ctrl Pts',(0.127861094297897,-0.0990616141723472,
1.27318980645355));
#16675=CARTESIAN_POINT('Ctrl Pts',(0.152546676219863,0.0537696421008814,
1.28113197457633));
#16676=CARTESIAN_POINT('Ctrl Pts',(0.0374838310097642,0.157342382244044,
1.28907414269911));
#16677=CARTESIAN_POINT('Ctrl Pts',(-0.111918054267102,0.116773335855419,
1.29701631082189));
#16678=CARTESIAN_POINT('Ctrl Pts',(-0.158791504053787,-0.0307720827589687,
1.30495847894467));
#16679=CARTESIAN_POINT('Ctrl Pts',(-0.060195622861772,-0.150127112226926,
1.31290064706745));
#16680=CARTESIAN_POINT('Ctrl Pts',(0.0935456330135535,-0.131950283756556,
1.32084281519023));
#16681=CARTESIAN_POINT('Ctrl Pts',(0.161589478720268,0.00710656041347678,
1.32878498331301));
#16682=CARTESIAN_POINT('Ctrl Pts',(0.0816007612396376,0.139653065139265,
1.33672715143579));
#16683=CARTESIAN_POINT('Ctrl Pts',(-0.0731426367739486,0.144263015132499,
1.34466931955857));
#16684=CARTESIAN_POINT('Ctrl Pts',(-0.160879865135934,0.0167132224867059,
1.35261148768135));
#16685=CARTESIAN_POINT('Ctrl Pts',(-0.101234609479067,-0.126147598829082,
1.36055365580413));
#16686=CARTESIAN_POINT('Ctrl Pts',(0.051151949184981,-0.153444260252591,
1.36849582392691));
#16687=CARTESIAN_POINT('Ctrl Pts',(0.15667806641111,-0.0401702148435725,
1.37643799204969));
#16688=CARTESIAN_POINT('Ctrl Pts',(0.118670980449659,0.10990387323047,1.38438016017247));
#16689=CARTESIAN_POINT('Ctrl Pts',(-0.0280509185434417,0.159294724422008,
1.39232232829525));
#16690=CARTESIAN_POINT('Ctrl Pts',(-0.149075287902345,0.0627552395607943,
1.40026449641803));
#16691=CARTESIAN_POINT('Ctrl Pts',(-0.133531390736797,-0.0912744851582948,
1.40820666454081));
#16692=CARTESIAN_POINT('Ctrl Pts',(0.00434100186018791,-0.161687417152987,
1.41614883266359));
#16693=CARTESIAN_POINT('Ctrl Pts',(0.138236546518021,-0.0839780402106489,
1.42409100078637));
#16694=CARTESIAN_POINT('Ctrl Pts',(0.145493297031458,0.07066380330362,1.43203316890915));
#16695=CARTESIAN_POINT('Ctrl Pts',(0.0194630807988606,0.160570430100525,
1.43997533703193));
#16696=CARTESIAN_POINT('Ctrl Pts',(-0.124397014000637,0.103377882332206,
1.44791750515471));
#16697=CARTESIAN_POINT('Ctrl Pts',(-0.15429723939393,-0.0485191136187331,
1.45585967327749));
#16698=CARTESIAN_POINT('Ctrl Pts',(-0.042844249846,-0.155968210152522,1.46380184140027));
#16699=CARTESIAN_POINT('Ctrl Pts',(0.107856400646442,-0.120533276677448,
1.47174400952305));
#16700=CARTESIAN_POINT('Ctrl Pts',(0.159753444358638,0.0253203827049868,
1.47968617764583));
#16701=CARTESIAN_POINT('Ctrl Pts',(0.0652924466007548,0.147982030257331,
1.48762834576861));
#16702=CARTESIAN_POINT('Ctrl Pts',(-0.0889689487809616,0.13506922671723,
1.49557051389139));
#16703=CARTESIAN_POINT('Ctrl Pts',(-0.161752593421533,-0.00156622680492735,
1.50351268201417));
#16704=CARTESIAN_POINT('Ctrl Pts',(-0.086303059730943,-0.136794666273195,
1.51145485013695));
#16705=CARTESIAN_POINT('Ctrl Pts',(0.0681115549116652,-0.14665217563879,
1.51939701825973));
#16706=CARTESIAN_POINT('Ctrl Pts',(0.160315645894948,-0.02226314405755,
1.52733918638251));
#16707=CARTESIAN_POINT('Ctrl Pts',(0.105284883301553,0.122726172858702,
1.53528135450529));
#16708=CARTESIAN_POINT('Ctrl Pts',(0.00484533846358528,0.144116573583224,
1.54057613325381));
#16709=CARTESIAN_POINT('Ctrl Pts',(-0.0388047044047284,0.131206995015745,
1.54322352262807));
#16710=CARTESIAN_POINT('Ctrl Pts',(-0.0634007094575145,0.131904027763688,
-3.88578058618805E-16));
#16711=CARTESIAN_POINT('Ctrl Pts',(-0.107282641710421,0.110811831533068,
0.00264738937425961));
#16712=CARTESIAN_POINT('Ctrl Pts',(-0.171581760589518,0.0217576868851663,
0.0079421681227796));
#16713=CARTESIAN_POINT('Ctrl Pts',(-0.111156590520044,-0.1327225175337,
0.0158843362455596));
#16714=CARTESIAN_POINT('Ctrl Pts',(0.0512451567233008,-0.165187689797298,
0.0238265043683396));
#16715=CARTESIAN_POINT('Ctrl Pts',(0.16662620135312,-0.0465387668729445,
0.0317686724911196));
#16716=CARTESIAN_POINT('Ctrl Pts',(0.129399745666171,0.114856349193662,
0.0397108406138996));
#16717=CARTESIAN_POINT('Ctrl Pts',(-0.026390801400978,0.170972456562021,
0.0476530087366796));
#16718=CARTESIAN_POINT('Ctrl Pts',(-0.157993800025737,0.070491178324729,
0.0555951768594596));
#16719=CARTESIAN_POINT('Ctrl Pts',(-0.144863967768493,-0.0945835600760224,
0.0635373449822396));
#16720=CARTESIAN_POINT('Ctrl Pts',(0.000979154756195248,-0.17300145605975,
0.0714795131050195));
#16721=CARTESIAN_POINT('Ctrl Pts',(0.145923683802689,-0.0929367665856833,
0.0794216812277997));
#16722=CARTESIAN_POINT('Ctrl Pts',(0.157187963117837,0.0722699302633024,
0.0873638493505794));
#16723=CARTESIAN_POINT('Ctrl Pts',(0.0244514793930555,0.171268692120756,
0.0953060174733598));
#16724=CARTESIAN_POINT('Ctrl Pts',(-0.130684839550095,0.113368397534175,
0.103248185596139));
#16725=CARTESIAN_POINT('Ctrl Pts',(-0.166100541844429,-0.0483893439312075,
0.11119035371892));
#16726=CARTESIAN_POINT('Ctrl Pts',(-0.0493510193195793,-0.165817291858885,
0.119132521841699));
#16727=CARTESIAN_POINT('Ctrl Pts',(0.112609073040783,-0.131339661914923,
0.12707468996448));
#16728=CARTESIAN_POINT('Ctrl Pts',(0.17140770357293,0.0234586422209967,
0.135016858087259));
#16729=CARTESIAN_POINT('Ctrl Pts',(0.0731792588499177,0.156766393306209,
0.14295902621004));
#16730=CARTESIAN_POINT('Ctrl Pts',(-0.0920889000195865,0.146460037003638,
0.150901194332819));
#16731=CARTESIAN_POINT('Ctrl Pts',(-0.172994168426659,0.00198123296575728,
0.1588433624556));
#16732=CARTESIAN_POINT('Ctrl Pts',(-0.0954190048152776,-0.144312580095855,
0.16678553057838));
#16733=CARTESIAN_POINT('Ctrl Pts',(0.0695697692503139,-0.158401246055831,
0.17472769870116));
#16734=CARTESIAN_POINT('Ctrl Pts',(0.170825487889685,-0.0273780963649298,
0.18266986682394));
#16735=CARTESIAN_POINT('Ctrl Pts',(0.115587509852263,0.128726201683253,
0.19061203494672));
#16736=CARTESIAN_POINT('Ctrl Pts',(-0.0455405018601966,0.16690407474553,
0.198554203069499));
#16737=CARTESIAN_POINT('Ctrl Pts',(-0.164948735370872,0.0521806684752238,
0.20649637119228));
#16738=CARTESIAN_POINT('Ctrl Pts',(-0.133246981425072,-0.110345590758605,
0.214438539315059));
#16739=CARTESIAN_POINT('Ctrl Pts',(0.0205226964731592,-0.171783952668295,
0.22238070743784));
#16740=CARTESIAN_POINT('Ctrl Pts',(0.155491476033395,-0.0758505658746651,
0.230322875560619));
#16741=CARTESIAN_POINT('Ctrl Pts',(0.148014089296488,0.0895697316726553,
0.2382650436834));
#16742=CARTESIAN_POINT('Ctrl Pts',(0.00494059070111224,0.172934953166096,
0.24620721180618));
#16743=CARTESIAN_POINT('Ctrl Pts',(-0.142658996543838,0.0978739912732451,
0.25414937992896));
#16744=CARTESIAN_POINT('Ctrl Pts',(-0.159568287038446,-0.0668496016012732,
0.262091548051739));
#16745=CARTESIAN_POINT('Ctrl Pts',(-0.0302966335331915,-0.170332091689456,
0.27003371617452));
#16746=CARTESIAN_POINT('Ctrl Pts',(0.126729848780061,-0.11777288690896,
0.2779758842973));
#16747=CARTESIAN_POINT('Ctrl Pts',(0.167658770158652,0.0426783815482623,
0.28591805242008));
#16748=CARTESIAN_POINT('Ctrl Pts',(0.0549950338320791,0.164031867990689,
0.293860220542859));
#16749=CARTESIAN_POINT('Ctrl Pts',(-0.108049803339193,0.135115311719503,
0.30180238866564));
#16750=CARTESIAN_POINT('Ctrl Pts',(-0.1721099202737,-0.0175807510100837,
0.309744556788419));
#16751=CARTESIAN_POINT('Ctrl Pts',(-0.0784996687135917,-0.154171039675278,
0.3176867249112));
#16752=CARTESIAN_POINT('Ctrl Pts',(0.087024343965547,-0.14952481740522,
0.325628893033979));
#16753=CARTESIAN_POINT('Ctrl Pts',(0.172825117221703,-0.00789850112384905,
0.33357106115676));
#16754=CARTESIAN_POINT('Ctrl Pts',(0.100300328103893,0.140963653630822,
0.341513229279539));
#16755=CARTESIAN_POINT('Ctrl Pts',(-0.0641098658012952,0.160688619913292,
0.349455397402319));
#16756=CARTESIAN_POINT('Ctrl Pts',(-0.16978883637574,0.033206302186043,
0.357397565525099));
#16757=CARTESIAN_POINT('Ctrl Pts',(-0.119923789760104,-0.124696399756661,
0.36533973364788));
#16758=CARTESIAN_POINT('Ctrl Pts',(0.0398037685148125,-0.168364388974385,
0.373281901770659));
#16759=CARTESIAN_POINT('Ctrl Pts',(0.163066985633654,-0.0577933011607096,
0.38122406989344));
#16760=CARTESIAN_POINT('Ctrl Pts',(0.136944091404129,0.10572238784759,0.38916623801622));
#16761=CARTESIAN_POINT('Ctrl Pts',(-0.0146336593526265,0.172385508313924,
0.397108406138999));
#16762=CARTESIAN_POINT('Ctrl Pts',(-0.152805474769431,0.0811257933285562,
0.40505057426178));
#16763=CARTESIAN_POINT('Ctrl Pts',(-0.150991776994562,-0.0844534827151793,
0.412992742384559));
#16764=CARTESIAN_POINT('Ctrl Pts',(-0.0108540995180527,-0.172664692355881,
0.42093491050734));
#16765=CARTESIAN_POINT('Ctrl Pts',(0.139227048201004,-0.102697305280782,
0.428877078630119));
#16766=CARTESIAN_POINT('Ctrl Pts',(0.16176191642983,0.0613513639265466,
0.4368192467529));
#16767=CARTESIAN_POINT('Ctrl Pts',(0.0361062507758455,0.169195880912067,
0.444761414875679));
#16768=CARTESIAN_POINT('Ctrl Pts',(-0.12262644992489,0.12203958882886,0.45270358299846));
#16769=CARTESIAN_POINT('Ctrl Pts',(-0.169020724600573,-0.0369175042249048,
0.460645751121239));
#16770=CARTESIAN_POINT('Ctrl Pts',(-0.0605746513833496,-0.162054370729346,
0.468587919244019));
#16771=CARTESIAN_POINT('Ctrl Pts',(0.103364025571403,-0.138732785167649,
0.4765300873668));
#16772=CARTESIAN_POINT('Ctrl Pts',(0.172610636112938,0.0116822841681558,
0.484472255489579));
#16773=CARTESIAN_POINT('Ctrl Pts',(0.083728171010617,0.151395181039277,
0.49241442361236));
#16774=CARTESIAN_POINT('Ctrl Pts',(-0.081857900459256,0.152414538660527,
0.500356591735139));
#16775=CARTESIAN_POINT('Ctrl Pts',(-0.172453725526818,0.0138065207282529,
0.50829875985792));
#16776=CARTESIAN_POINT('Ctrl Pts',(-0.105064221167447,-0.137449688588867,
0.516240927980699));
#16777=CARTESIAN_POINT('Ctrl Pts',(0.0585749034388466,-0.162787862415564,
0.52418309610348));
#16778=CARTESIAN_POINT('Ctrl Pts',(0.168553398866689,-0.0389956304370821,
0.532125264226259));
#16779=CARTESIAN_POINT('Ctrl Pts',(0.124119664784058,0.120520605195094,
0.54006743234904));
#16780=CARTESIAN_POINT('Ctrl Pts',(-0.0340204335384149,0.16962758491636,
0.548009600471819));
#16781=CARTESIAN_POINT('Ctrl Pts',(-0.160994319687769,0.0633382703503284,
0.5559517685946));
#16782=CARTESIAN_POINT('Ctrl Pts',(-0.14048086942825,-0.100975406844349,
0.563893936717379));
#16783=CARTESIAN_POINT('Ctrl Pts',(0.00872748937560605,-0.172785237771916,
0.57183610484016));
#16784=CARTESIAN_POINT('Ctrl Pts',(0.149940571302356,-0.0863060399984934,
0.579778272962939));
#16785=CARTESIAN_POINT('Ctrl Pts',(0.153792685935992,0.0792383569699183,
0.58772044108572));
#16786=CARTESIAN_POINT('Ctrl Pts',(0.0167549005293281,0.17219227848818,
0.595662609208499));
#16787=CARTESIAN_POINT('Ctrl Pts',(-0.135632095058532,0.107400382926376,
0.60360477733128));
#16788=CARTESIAN_POINT('Ctrl Pts',(-0.163766157558233,-0.0557812970565469,
0.611546945454059));
#16789=CARTESIAN_POINT('Ctrl Pts',(-0.0418735953979919,-0.167861578305293,
0.61948911357684));
#16790=CARTESIAN_POINT('Ctrl Pts',(0.118379481984711,-0.126163408751231,
0.627431281699619));
#16791=CARTESIAN_POINT('Ctrl Pts',(0.17018479228316,0.0311134044783985,
0.6353734498224));
#16792=CARTESIAN_POINT('Ctrl Pts',(0.0660833491022344,0.159887142804326,
0.643315617945179));
#16793=CARTESIAN_POINT('Ctrl Pts',(-0.0985572308567358,0.142187832491218,
0.651257786067961));
#16794=CARTESIAN_POINT('Ctrl Pts',(-0.172909262181909,-0.00577013989488307,
0.659199954190738));
#16795=CARTESIAN_POINT('Ctrl Pts',(-0.0888586457050277,-0.148442071348278,
0.667142122313521));
#16796=CARTESIAN_POINT('Ctrl Pts',(0.0765956190331784,-0.155125815413241,
0.675084290436298));
#16797=CARTESIAN_POINT('Ctrl Pts',(0.171880427770071,-0.0196983758791502,
0.683026458559081));
#16798=CARTESIAN_POINT('Ctrl Pts',(0.109705106722326,0.133774799651286,
0.690968626681858));
#16799=CARTESIAN_POINT('Ctrl Pts',(-0.0529713625168984,0.164696515493808,
0.698910794804641));
#16800=CARTESIAN_POINT('Ctrl Pts',(-0.167120621735807,0.0447393032280997,
0.706852962927418));
#16801=CARTESIAN_POINT('Ctrl Pts',(-0.12817022249092,-0.116203707037801,
0.7147951310502));
#16802=CARTESIAN_POINT('Ctrl Pts',(0.0281972679828983,-0.17069218359667,
0.722737299172979));
#16803=CARTESIAN_POINT('Ctrl Pts',(0.158733164168978,-0.0688090841067,0.73067946729576));
#16804=CARTESIAN_POINT('Ctrl Pts',(0.14385317469873,0.0961102054508026,
0.738621635418538));
#16805=CARTESIAN_POINT('Ctrl Pts',(-0.00281110139369983,0.172982673038814,
0.746563803541321));
#16806=CARTESIAN_POINT('Ctrl Pts',(-0.146900119814081,0.0913852409380608,
0.754505971664098));
#16807=CARTESIAN_POINT('Ctrl Pts',(-0.156413536862055,-0.0739304602244656,
0.762448139786881));
#16808=CARTESIAN_POINT('Ctrl Pts',(-0.0226360851712103,-0.171518264656626,
0.770390307909658));
#16809=CARTESIAN_POINT('Ctrl Pts',(0.131878346029848,-0.111977717922496,
0.778332476032441));
#16810=CARTESIAN_POINT('Ctrl Pts',(0.165578663890314,0.0501459223366878,
0.786274644155218));
#16811=CARTESIAN_POINT('Ctrl Pts',(0.047591915084802,0.166330746049129,
0.794216812278001));
#16812=CARTESIAN_POINT('Ctrl Pts',(-0.113993917241593,0.130139518573781,
0.802158980400778));
#16813=CARTESIAN_POINT('Ctrl Pts',(-0.171149610334614,-0.0252728776558711,
0.81010114852356));
#16814=CARTESIAN_POINT('Ctrl Pts',(-0.0715146774936035,-0.157532721571376,
0.818043316646339));
#16815=CARTESIAN_POINT('Ctrl Pts',(0.0936350469135118,-0.14547640857611,
0.825985484769119));
#16816=CARTESIAN_POINT('Ctrl Pts',(0.173005448853992,-0.000148759965830227,
0.8339276528919));
#16817=CARTESIAN_POINT('Ctrl Pts',(0.0938850861191564,0.145315168055841,
0.841869821014678));
#16818=CARTESIAN_POINT('Ctrl Pts',(-0.0712436606821878,0.157655473343934,
0.849811989137461));
#16819=CARTESIAN_POINT('Ctrl Pts',(-0.171105895159299,0.0255671684868261,
0.857754157260238));
#16820=CARTESIAN_POINT('Ctrl Pts',(-0.114217551294,-0.129943289319231,0.86569632538302));
#16821=CARTESIAN_POINT('Ctrl Pts',(0.0473058035714782,-0.166412344527548,
0.873638493505798));
#16822=CARTESIAN_POINT('Ctrl Pts',(0.16549218245563,-0.0504305959589149,
0.88158066162858));
#16823=CARTESIAN_POINT('Ctrl Pts',(0.132070720552549,0.111750759440056,
0.889522829751358));
#16824=CARTESIAN_POINT('Ctrl Pts',(-0.022341089517305,0.171556938600217,
0.89746499787414));
#16825=CARTESIAN_POINT('Ctrl Pts',(-0.156286166401977,0.074199337288632,
0.905407165996919));
#16826=CARTESIAN_POINT('Ctrl Pts',(-0.147057058974526,-0.0911324797668838,
0.913349334119699));
#16827=CARTESIAN_POINT('Ctrl Pts',(-0.00310857778072832,-0.172977582960567,
0.92129150224248));
#16828=CARTESIAN_POINT('Ctrl Pts',(0.143687680016546,-0.0963574495000853,
0.929233670365259));
#16829=CARTESIAN_POINT('Ctrl Pts',(0.158851261322436,0.0685360068793772,
0.93717583848804));
#16830=CARTESIAN_POINT('Ctrl Pts',(0.0284907678468484,0.170643439985825,
0.945118006610819));
#16831=CARTESIAN_POINT('Ctrl Pts',(-0.127970195944242,0.116423951198588,
0.9530601747336));
#16832=CARTESIAN_POINT('Ctrl Pts',(-0.167197313372666,-0.0444518375735043,
0.961002342856378));
#16833=CARTESIAN_POINT('Ctrl Pts',(-0.0532545149190986,-0.164605176417482,
0.96894451097916));
#16834=CARTESIAN_POINT('Ctrl Pts',(0.10947489024455,-0.133963263130763,
0.976886679101939));
#16835=CARTESIAN_POINT('Ctrl Pts',(0.1719140491614,0.0194027617526574,0.984828847224719));
#16836=CARTESIAN_POINT('Ctrl Pts',(0.0768622776450996,0.154993863549195,
0.992771015347499));
#16837=CARTESIAN_POINT('Ctrl Pts',(-0.088603236555915,0.148594663210074,
1.00071318347028));
#16838=CARTESIAN_POINT('Ctrl Pts',(-0.172899083515371,0.00606748566075909,
1.00865535159306));
#16839=CARTESIAN_POINT('Ctrl Pts',(-0.0988016073770141,-0.142018132090297,
1.01659751971584));
#16840=CARTESIAN_POINT('Ctrl Pts',(0.0658082913934689,-0.160000550769587,
1.02453968783862));
#16841=CARTESIAN_POINT('Ctrl Pts',(0.170131034504888,-0.0314060274628177,
1.0324818559614));
#16842=CARTESIAN_POINT('Ctrl Pts',(0.118596271784576,0.125959643463681,
1.04042402408418));
#16843=CARTESIAN_POINT('Ctrl Pts',(-0.0415848597483297,0.167933340651612,
1.04836619220696));
#16844=CARTESIAN_POINT('Ctrl Pts',(-0.163669987576804,0.0560628453550813,
1.05630836032974));
#16845=CARTESIAN_POINT('Ctrl Pts',(-0.135816592328243,-0.107166975841641,
1.06425052845252));
#16846=CARTESIAN_POINT('Ctrl Pts',(0.0164587544616562,-0.172220837485682,
1.0721926965753));
#16847=CARTESIAN_POINT('Ctrl Pts',(0.153656191292587,-0.0795027190739688,
1.08013486469808));
#16848=CARTESIAN_POINT('Ctrl Pts',(0.150088771199207,0.0860480576341552,
1.08807703282086));
#16849=CARTESIAN_POINT('Ctrl Pts',(0.00902461748204118,0.172769973496559,
1.09601920094364));
#16850=CARTESIAN_POINT('Ctrl Pts',(-0.140307012982855,0.101216844302358,
1.10396136906642));
#16851=CARTESIAN_POINT('Ctrl Pts',(-0.161103005268346,-0.0630613126743013,
1.1119035371892));
#16852=CARTESIAN_POINT('Ctrl Pts',(-0.0343120939874615,-0.1695688287065,
1.11984570531198));
#16853=CARTESIAN_POINT('Ctrl Pts',(0.123912220401285,-0.120733877175888,
1.12778787343476));
#16854=CARTESIAN_POINT('Ctrl Pts',(0.168620210916381,0.0387057093103061,
1.13573004155754));
#16855=CARTESIAN_POINT('Ctrl Pts',(0.0588547652196237,0.162686889679659,
1.14367220968032));
#16856=CARTESIAN_POINT('Ctrl Pts',(-0.104827691798069,0.137630165643247,
1.1516143778031));
#16857=CARTESIAN_POINT('Ctrl Pts',(-0.172477213770776,-0.0135099294065116,
1.15955654592588));
#16858=CARTESIAN_POINT('Ctrl Pts',(-0.0821198886720452,-0.152273541192125,
1.16749871404866));
#16859=CARTESIAN_POINT('Ctrl Pts',(0.083467690946984,-0.15153894559049,
1.17544088217144));
#16860=CARTESIAN_POINT('Ctrl Pts',(0.172590290696882,-0.0119791076405788,
1.18338305029422));
#16861=CARTESIAN_POINT('Ctrl Pts',(0.103602453294194,0.13855482356859,1.191325218417));
#16862=CARTESIAN_POINT('Ctrl Pts',(-0.0602958748103966,0.162158302111078,
1.19926738653978));
#16863=CARTESIAN_POINT('Ctrl Pts',(-0.168956987158091,0.0372081167644847,
1.20720955466256));
#16864=CARTESIAN_POINT('Ctrl Pts',(-0.122836141658186,-0.121828526073448,
1.21515172278534));
#16865=CARTESIAN_POINT('Ctrl Pts',(0.0358152290369173,-0.169257723108079,
1.22309389090812));
#16866=CARTESIAN_POINT('Ctrl Pts',(0.161656170495932,-0.0616294572691503,
1.2310360590309));
#16867=CARTESIAN_POINT('Ctrl Pts',(0.13940345221127,0.102457722863032,1.23897822715368));
#16868=CARTESIAN_POINT('Ctrl Pts',(-0.0105571497596809,0.172683102970871,
1.24692039527646));
#16869=CARTESIAN_POINT('Ctrl Pts',(-0.150846317973597,0.0847130203482025,
1.25486256339924));
#16870=CARTESIAN_POINT('Ctrl Pts',(-0.152944761892581,-0.0808628918127005,
1.26280473152202));
#16871=CARTESIAN_POINT('Ctrl Pts',(-0.0149300913057054,-0.172360087712588,
1.2707468996448));
#16872=CARTESIAN_POINT('Ctrl Pts',(0.136762076743997,-0.105957736043287,
1.27868906776758));
#16873=CARTESIAN_POINT('Ctrl Pts',(0.163166132393764,0.0575127872937276,
1.28663123589036));
#16874=CARTESIAN_POINT('Ctrl Pts',(0.0400932480780463,0.168295688956082,
1.29457340401314));
#16875=CARTESIAN_POINT('Ctrl Pts',(-0.119709170414695,0.124902449862528,
1.30251557213592));
#16876=CARTESIAN_POINT('Ctrl Pts',(-0.169845690614082,-0.0329142650230248,
1.3104577402587));
#16877=CARTESIAN_POINT('Ctrl Pts',(-0.0643861093061943,-0.160578131733314,
1.31839990838148));
#16878=CARTESIAN_POINT('Ctrl Pts',(0.100057762773863,-0.141135932963798,
1.32634207650426));
#16879=CARTESIAN_POINT('Ctrl Pts',(0.172838444806952,0.00760127985757451,
1.33428424462704));
#16880=CARTESIAN_POINT('Ctrl Pts',(0.0872813550697656,0.149374939398002,
1.34222641274982));
#16881=CARTESIAN_POINT('Ctrl Pts',(-0.0782344227434143,0.154305808621531,
1.3501685808726));
#16882=CARTESIAN_POINT('Ctrl Pts',(-0.172079431848303,0.0178767046294837,
1.35811074899538));
#16883=CARTESIAN_POINT('Ctrl Pts',(-0.108282003268856,-0.134929297194493,
1.36605291711816));
#16884=CARTESIAN_POINT('Ctrl Pts',(0.0547128650701426,-0.164126201264144,
1.37399508524094));
#16885=CARTESIAN_POINT('Ctrl Pts',(0.167585127127835,-0.0429666431014547,
1.38193725336372));
#16886=CARTESIAN_POINT('Ctrl Pts',(0.126932197981417,0.117554773230619,
1.3898794214865));
#16887=CARTESIAN_POINT('Ctrl Pts',(-0.0300036684000219,0.170383942402052,
1.39782158960928));
#16888=CARTESIAN_POINT('Ctrl Pts',(-0.159453085214751,0.0671239123677834,
1.40576375773206));
#16889=CARTESIAN_POINT('Ctrl Pts',(-0.142827107870127,-0.0976285101620078,
1.41370592585484));
#16890=CARTESIAN_POINT('Ctrl Pts',(0.00464319840846943,-0.172943201171859,
1.42164809397762));
#16891=CARTESIAN_POINT('Ctrl Pts',(0.147859810582222,-0.0898241270588577,
1.4295902621004));
#16892=CARTESIAN_POINT('Ctrl Pts',(0.155621735944117,0.0755830265922534,
1.43753243022318));
#16893=CARTESIAN_POINT('Ctrl Pts',(0.0208179928734729,0.171748455656582,
1.44547459834596));
#16894=CARTESIAN_POINT('Ctrl Pts',(-0.133056846329205,0.11057447892796,
1.45341676646874));
#16895=CARTESIAN_POINT('Ctrl Pts',(-0.165038560097216,-0.0518967460486161,
1.46135893459152));
#16896=CARTESIAN_POINT('Ctrl Pts',(-0.0458268296361176,-0.166825854601292,
1.4693011027143));
#16897=CARTESIAN_POINT('Ctrl Pts',(0.115364766925686,-0.128924136976022,
1.47724327083708));
#16898=CARTESIAN_POINT('Ctrl Pts',(0.170874595884426,0.0270830477535184,
1.48518543895986));
#16899=CARTESIAN_POINT('Ctrl Pts',(0.0698377457337486,0.158283721017069,
1.49312760708264));
#16900=CARTESIAN_POINT('Ctrl Pts',(-0.0951624750893037,0.144471999488883,
1.50106977520542));
#16901=CARTESIAN_POINT('Ctrl Pts',(-0.173012914651864,-0.00167525885548286,
1.5090119433282));
#16902=CARTESIAN_POINT('Ctrl Pts',(-0.092311001583214,-0.14631755460685,
1.51695411145098));
#16903=CARTESIAN_POINT('Ctrl Pts',(0.072853104778531,-0.156861289272697,
1.52489627957376));
#16904=CARTESIAN_POINT('Ctrl Pts',(0.171475934783304,-0.0238129810547936,
1.53283844769654));
#16905=CARTESIAN_POINT('Ctrl Pts',(0.11261423476106,0.131269690464983,1.54078061581932));
#16906=CARTESIAN_POINT('Ctrl Pts',(0.00518264413773371,0.154149172621267,
1.54607539456784));
#16907=CARTESIAN_POINT('Ctrl Pts',(-0.0415060733757155,0.140340900570467,
1.5487227839421));
#16908=CARTESIAN_POINT('Ctrl Pts',(-0.146248097568756,-0.000123763188177425,
1.45893449541571));
#16909=CARTESIAN_POINT('Ctrl Pts',(-0.146367493381718,-0.0150081347743067,
1.45974264180765));
#16910=CARTESIAN_POINT('Ctrl Pts',(-0.144277648885518,-0.0298597803798721,
1.46055078819958));
#16911=CARTESIAN_POINT('Ctrl Pts',(-0.139839652725699,-0.043973059977961,
1.46135893459152));
#16912=CARTESIAN_POINT('Ctrl Pts',(-0.125301316610186,-0.0902064488995044,
1.46400632396578));
#16913=CARTESIAN_POINT('Ctrl Pts',(-0.08556407312315,-0.1285161517504,1.46665371334004));
#16914=CARTESIAN_POINT('Ctrl Pts',(-0.0388301852859989,-0.141354050238301,
1.4693011027143));
#16915=CARTESIAN_POINT('Ctrl Pts',(0.00790370255115092,-0.154191948726202,
1.47194849208856));
#16916=CARTESIAN_POINT('Ctrl Pts',(0.0616342347384179,-0.141558042851112,
1.47459588146282));
#16917=CARTESIAN_POINT('Ctrl Pts',(0.0977511389918415,-0.109239892458645,
1.47724327083708));
#16918=CARTESIAN_POINT('Ctrl Pts',(0.133868043245265,-0.0769217420661769,
1.47989066021134));
#16919=CARTESIAN_POINT('Ctrl Pts',(0.152371319564846,-0.024919347156331,
1.4825380495856));
#16920=CARTESIAN_POINT('Ctrl Pts',(0.144783482699524,0.0229486291758506,
1.48518543895986));
#16921=CARTESIAN_POINT('Ctrl Pts',(0.137195645834202,0.0708166055080336,
1.48783282833412));
#16922=CARTESIAN_POINT('Ctrl Pts',(0.103516695783975,0.114550163262552,
1.49048021770838));
#16923=CARTESIAN_POINT('Ctrl Pts',(0.0591771839550196,0.13411498855178,
1.49312760708264));
#16924=CARTESIAN_POINT('Ctrl Pts',(0.014837672126065,0.153679813841007,
1.4957749964569));
#16925=CARTESIAN_POINT('Ctrl Pts',(-0.0401624014816186,0.149075906664945,
1.49842238583116));
#16926=CARTESIAN_POINT('Ctrl Pts',(-0.0806375115458872,0.122416076686187,
1.50106977520542));
#16927=CARTESIAN_POINT('Ctrl Pts',(-0.0937869288003098,0.113754921033589,
1.50192985013695));
#16928=CARTESIAN_POINT('Ctrl Pts',(-0.105403311347291,0.102765876910903,
1.50278992506847));
#16929=CARTESIAN_POINT('Ctrl Pts',(-0.115078604842433,0.0902138214954038,
1.50365));
#16930=CARTESIAN_POINT('Ctrl Pts',(-0.0686146973663081,-0.0959584553529135,
1.07336015076065E-17));
#16931=CARTESIAN_POINT('Ctrl Pts',(-0.0712979561985307,-0.0944995001033786,
9.02613639135873E-18));
#16932=CARTESIAN_POINT('Ctrl Pts',(-0.0739152333025289,-0.0929325179580126,
1.64107321374712E-17));
#16933=CARTESIAN_POINT('Ctrl Pts',(-0.0764591723283171,-0.0912589988675934,
1.6154612370034E-17));
#16934=CARTESIAN_POINT('Ctrl Pts',(-0.0824897891353913,-0.0872917841461184,
1.52077426268717E-17));
#16935=CARTESIAN_POINT('Ctrl Pts',(-0.0881090519769445,-0.0827275518978924,
1.30971627060498E-17));
#16936=CARTESIAN_POINT('Ctrl Pts',(-0.0932912133381108,-0.0776621329443405,
1.43114686768087E-17));
#16937=CARTESIAN_POINT('Ctrl Pts',(-0.0960634919631888,-0.074952307504085,
1.49610807310118E-17));
#16938=CARTESIAN_POINT('Ctrl Pts',(-0.0987043519497191,-0.0721043812799658,
1.74993329480528E-17));
#16939=CARTESIAN_POINT('Ctrl Pts',(-0.101206237074718,-0.0691378820326018,
9.97465998686664E-18));
#16940=CARTESIAN_POINT('Ctrl Pts',(-0.105823426721714,-0.0636632543305198,
-3.91200561030858E-18));
#16941=CARTESIAN_POINT('Ctrl Pts',(-0.109972666997065,-0.0577811896139199,
2.24798207762934E-18));
#16942=CARTESIAN_POINT('Ctrl Pts',(-0.113625452403263,-0.0515741981665521,
9.54097911787244E-18));
#16943=CARTESIAN_POINT('Ctrl Pts',(-0.115386295340069,-0.0485820878086944,
1.30566037435822E-17));
#16944=CARTESIAN_POINT('Ctrl Pts',(-0.117027309103105,-0.0455212415157476,
-2.79521757168051E-18));
#16945=CARTESIAN_POINT('Ctrl Pts',(-0.118543833519887,-0.0424058589801268,
-3.46944695195361E-18));
#16946=CARTESIAN_POINT('Ctrl Pts',(-0.122700941917732,-0.0338659484069709,
-5.31764971597768E-18));
#16947=CARTESIAN_POINT('Ctrl Pts',(-0.125931492798984,-0.0249085743588085,
-1.15219401683824E-18));
#16948=CARTESIAN_POINT('Ctrl Pts',(-0.128167520083254,-0.0157105262534848,
9.54097911787244E-18));
#16949=CARTESIAN_POINT('Ctrl Pts',(-0.128992166906242,-0.0123182862745252,
1.3484621181291E-17));
#16950=CARTESIAN_POINT('Ctrl Pts',(-0.129681150280034,-0.00889298553317688,
1.10989611676181E-17));
#16951=CARTESIAN_POINT('Ctrl Pts',(-0.130229483957028,-0.00544263935519351,
9.54097911787244E-18));
#16952=CARTESIAN_POINT('Ctrl Pts',(-0.130761899349706,-0.00209245771889707,
8.02822573502553E-18));
#16953=CARTESIAN_POINT('Ctrl Pts',(-0.131160261982709,0.00127366115726457,
1.11791151702242E-17));
#16954=CARTESIAN_POINT('Ctrl Pts',(-0.131420990891747,0.00464012593483382,
8.67361737988404E-18));
#16955=CARTESIAN_POINT('Ctrl Pts',(-0.131728666658755,0.00861275649723166,
5.71697955546795E-18));
#16956=CARTESIAN_POINT('Ctrl Pts',(-0.131845259942619,0.0125891451047215,
-9.26473565962443E-18));
#16957=CARTESIAN_POINT('Ctrl Pts',(-0.131765781147177,0.0165567997877194,
-1.04083408558608E-17));
#16958=CARTESIAN_POINT('Ctrl Pts',(-0.131635692412819,0.0230509492424239,
-1.21888544026837E-17));
#16959=CARTESIAN_POINT('Ctrl Pts',(-0.13098103789945,0.0295216962360144,
-2.67049856555875E-17));
#16960=CARTESIAN_POINT('Ctrl Pts',(-0.129839098367345,0.0359278479980343,
-3.46944695195361E-17));
#16961=CARTESIAN_POINT('Ctrl Pts',(-0.129254890951344,0.0392051855997028,
-3.87818275556788E-17));
#16962=CARTESIAN_POINT('Ctrl Pts',(-0.128542951403208,0.0424656461998481,
-3.10678831811161E-17));
#16963=CARTESIAN_POINT('Ctrl Pts',(-0.1277070993652,0.0457037274559979,
-3.29597460435593E-17));
#16964=CARTESIAN_POINT('Ctrl Pts',(-0.126886363095037,0.0488832504000222,
-3.48173959609792E-17));
#16965=CARTESIAN_POINT('Ctrl Pts',(-0.125948031872817,0.0520333657183593,
-3.53366201082739E-17));
#16966=CARTESIAN_POINT('Ctrl Pts',(-0.124899042599898,0.0551436241923499,
-3.46944695195361E-17));
#16967=CARTESIAN_POINT('Ctrl Pts',(-0.122234979928128,0.0630425834229368,
-3.30636335736642E-17));
#16968=CARTESIAN_POINT('Ctrl Pts',(-0.118856305871375,0.070695441500891,
-2.1366080483524E-17));
#16969=CARTESIAN_POINT('Ctrl Pts',(-0.114834854776346,0.078019637496205,
-1.73472347597681E-17));
#16970=CARTESIAN_POINT('Ctrl Pts',(-0.11215901866562,0.0828930893082948,
-1.46731322388254E-17));
#16971=CARTESIAN_POINT('Ctrl Pts',(-0.109198005187061,0.0876211033078822,
8.28606628989234E-18));
#16972=CARTESIAN_POINT('Ctrl Pts',(-0.105966883726074,0.0921780034666525,
8.67361737988404E-18));
#16973=CARTESIAN_POINT('Ctrl Pts',(-0.104137243112614,0.094758373688769,
8.89307035390601E-18));
#16974=CARTESIAN_POINT('Ctrl Pts',(-0.102221042121924,0.0972831505018574,
-2.31209379389524E-17));
#16975=CARTESIAN_POINT('Ctrl Pts',(-0.100229777791505,0.0997373632832089,
-2.08166817117217E-17));
#16976=CARTESIAN_POINT('Ctrl Pts',(-0.0937202782075859,0.107760254486057,
-1.32840027382311E-17));
#16977=CARTESIAN_POINT('Ctrl Pts',(-0.0863914655699752,0.115060936709644,
5.4842312373535E-18));
#16978=CARTESIAN_POINT('Ctrl Pts',(-0.0783508402622743,0.121487309774744,
1.38777878078145E-17));
#16979=CARTESIAN_POINT('Ctrl Pts',(-0.073610711791116,0.125275800441382,
1.8825977152717E-17));
#16980=CARTESIAN_POINT('Ctrl Pts',(-0.068622257850438,0.128760167547443,
-9.09579695168528E-18));
#16981=CARTESIAN_POINT('Ctrl Pts',(-0.0634007094575209,0.131904027763685,
-6.93889390390723E-18));
#16982=CARTESIAN_POINT('Origin',(0.,0.,0.));
#16983=CARTESIAN_POINT('Origin',(-0.0721687836487033,-0.125,-0.3));
#16984=CARTESIAN_POINT('',(-0.0721687836487033,-0.125,-0.3));
#16985=CARTESIAN_POINT('',(0.0721687836487032,-0.125,-0.3));
#16986=CARTESIAN_POINT('',(-0.0360843918243517,-0.125,-0.3));
#16987=CARTESIAN_POINT('',(-0.0721687836487033,-0.125,-0.15));
#16988=CARTESIAN_POINT('',(-0.0721687836487033,-0.125,-0.3));
#16989=CARTESIAN_POINT('',(0.0721687836487032,-0.125,-0.15));
#16990=CARTESIAN_POINT('',(-0.0721687836487033,-0.125,-0.15));
#16991=CARTESIAN_POINT('',(0.0721687836487032,-0.125,-0.3));
#16992=CARTESIAN_POINT('Origin',(-0.144337567297406,1.76762539787485E-17,
-0.3));
#16993=CARTESIAN_POINT('',(-0.144337567297406,1.76762539787485E-17,-0.3));
#16994=CARTESIAN_POINT('',(-0.126295371385231,-0.03125,-0.3));
#16995=CARTESIAN_POINT('',(-0.144337567297406,2.77555756156289E-17,-0.15));
#16996=CARTESIAN_POINT('',(-0.144337567297406,1.76762539787485E-17,-0.3));
#16997=CARTESIAN_POINT('',(-0.144337567297406,1.76762539787485E-17,-0.15));
#16998=CARTESIAN_POINT('Origin',(-0.0721687836487032,0.125,-0.3));
#16999=CARTESIAN_POINT('',(-0.0721687836487032,0.125,-0.3));
#17000=CARTESIAN_POINT('',(-0.090210979560879,0.09375,-0.3));
#17001=CARTESIAN_POINT('',(-0.0721687836487032,0.125,-0.15));
#17002=CARTESIAN_POINT('',(-0.0721687836487032,0.125,-0.3));
#17003=CARTESIAN_POINT('',(-0.0721687836487032,0.125,-0.15));
#17004=CARTESIAN_POINT('Origin',(0.0721687836487032,0.125,-0.3));
#17005=CARTESIAN_POINT('',(0.0721687836487032,0.125,-0.3));
#17006=CARTESIAN_POINT('',(0.0360843918243516,0.125,-0.3));
#17007=CARTESIAN_POINT('',(0.0721687836487032,0.125,-0.15));
#17008=CARTESIAN_POINT('',(0.0721687836487032,0.125,-0.3));
#17009=CARTESIAN_POINT('',(0.0721687836487032,0.125,-0.15));
#17010=CARTESIAN_POINT('Origin',(0.144337567297406,0.,-0.3));
#17011=CARTESIAN_POINT('',(0.144337567297406,0.,-0.3));
#17012=CARTESIAN_POINT('',(0.126295371385231,0.03125,-0.3));
#17013=CARTESIAN_POINT('',(0.144337567297406,0.,-0.15));
#17014=CARTESIAN_POINT('',(0.144337567297406,0.,-0.3));
#17015=CARTESIAN_POINT('',(0.144337567297406,0.,-0.15));
#17016=CARTESIAN_POINT('Origin',(0.0721687836487032,-0.125,-0.3));
#17017=CARTESIAN_POINT('',(0.0902109795608791,-0.09375,-0.3));
#17018=CARTESIAN_POINT('',(0.0721687836487032,-0.125,-0.15));
#17019=CARTESIAN_POINT('Origin',(0.,0.,-0.15));
#17020=CARTESIAN_POINT('Origin',(0.,0.,0.));
#17021=CARTESIAN_POINT('',(-0.275,-3.36777869765522E-17,0.));
#17022=CARTESIAN_POINT('Origin',(0.,0.,0.));
#17023=CARTESIAN_POINT('Origin',(0.,0.,-0.3));
#17024=CARTESIAN_POINT('',(-0.275,-3.36777869765522E-17,-0.3));
#17025=CARTESIAN_POINT('',(-0.275,-3.36777869765522E-17,-0.3));
#17026=CARTESIAN_POINT('Origin',(0.,0.,-0.3));
#17027=CARTESIAN_POINT('Origin',(0.,0.,-0.3));
#17028=CARTESIAN_POINT('Origin',(0.,0.,1.6));
#17029=CARTESIAN_POINT('',(0.,0.,0.));
#17030=CARTESIAN_POINT('Origin',(0.,0.,0.12));
#17031=CARTESIAN_POINT('',(-0.12639138516214,8.91322620741042E-5,0.00934196736194174));
#17032=CARTESIAN_POINT('',(-0.12645,1.54856587752183E-17,-5.55111512312578E-17));
#17033=CARTESIAN_POINT('',(-0.12645,1.54856587752183E-17,0.12));
#17034=CARTESIAN_POINT('',(-0.0488748409397564,0.116622692573588,0.));
#17035=CARTESIAN_POINT('Origin',(0.,0.,0.));
#17036=CARTESIAN_POINT('Ctrl Pts',(-0.0489111879062984,0.116810626195002,
1.20007714660797E-17));
#17037=CARTESIAN_POINT('Ctrl Pts',(-0.0838963038512042,0.101957324585112,
0.00240024091002088));
#17038=CARTESIAN_POINT('Ctrl Pts',(-0.11198221847721,0.0702793053867637,
0.00480048182004174));
#17039=CARTESIAN_POINT('Ctrl Pts',(-0.122072221370749,0.0336561163696377,
0.00720072273006261));
#17040=CARTESIAN_POINT('Ctrl Pts',(-0.125072637487486,0.022765653033531,
0.00791447094068899));
#17041=CARTESIAN_POINT('Ctrl Pts',(-0.126481745582665,0.0114379076904012,
0.00862821915131536));
#17042=CARTESIAN_POINT('Ctrl Pts',(-0.12639138516214,8.91322620741042E-5,
0.00934196736194174));
#17043=CARTESIAN_POINT('Origin',(0.,0.,0.12));
#17044=CARTESIAN_POINT('',(-0.126396145829628,-9.95859796292312E-5,0.0593419673619417));
#17045=CARTESIAN_POINT('',(-0.126575671592806,-7.20628672610732E-5,0.0456580326380584));
#17046=CARTESIAN_POINT('',(-0.12645,1.54856587752183E-17,0.12));
#17047=CARTESIAN_POINT('',(-0.10808967569503,-0.0656218295092665,0.));
#17048=CARTESIAN_POINT('Ctrl Pts',(-0.126575671592806,-7.20628672610732E-5,
0.0456580326380584));
#17049=CARTESIAN_POINT('Ctrl Pts',(-0.126327459688109,0.0361497101693465,
0.0433719816070355));
#17050=CARTESIAN_POINT('Ctrl Pts',(-0.109912066394173,0.0725710138228805,
0.0410859305760125));
#17051=CARTESIAN_POINT('Ctrl Pts',(-0.0824515099939393,0.0961223418729112,
0.0387998795449896));
#17052=CARTESIAN_POINT('Ctrl Pts',(-0.05137998778939,0.122770586059505,
0.036213220908657));
#17053=CARTESIAN_POINT('Ctrl Pts',(-0.00616751748104999,0.132941603485868,
0.0336265622723243));
#17054=CARTESIAN_POINT('Ctrl Pts',(0.0333172074018229,0.122176268745047,
0.0310399036359917));
#17055=CARTESIAN_POINT('Ctrl Pts',(0.0728019322846963,0.111410934004226,
0.028453244999659));
#17056=CARTESIAN_POINT('Ctrl Pts',(0.106558911742102,0.0797092470962188,
0.0258665863633264));
#17057=CARTESIAN_POINT('Ctrl Pts',(0.11981357554495,0.0409763259700822,
0.0232799277269937));
#17058=CARTESIAN_POINT('Ctrl Pts',(0.133068239347797,0.00224340484394604,
0.0206932690906611));
#17059=CARTESIAN_POINT('Ctrl Pts',(0.125820587496086,-0.0435207505003201,
0.0181066104543285));
#17060=CARTESIAN_POINT('Ctrl Pts',(0.101166903546451,-0.0762076816581678,
0.0155199518179958));
#17061=CARTESIAN_POINT('Ctrl Pts',(0.0765132195968157,-0.108894612816016,
0.0129332931816632));
#17062=CARTESIAN_POINT('Ctrl Pts',(0.0344535035492562,-0.128504319787445,
0.0103466345453306));
#17063=CARTESIAN_POINT('Ctrl Pts',(-0.00636464094143544,-0.126469737202777,
0.00775997590899791));
#17064=CARTESIAN_POINT('Ctrl Pts',(-0.0471827854321269,-0.124435154618108,
0.00517331727266527));
#17065=CARTESIAN_POINT('Ctrl Pts',(-0.0867593583659505,-0.100756282477341,
0.00258665863633259));
#17066=CARTESIAN_POINT('Ctrl Pts',(-0.108089675695031,-0.0656218295092657,
-5.55111512312578E-17));
#17067=CARTESIAN_POINT('Origin',(0.,0.,0.));
#17068=CARTESIAN_POINT('Ctrl Pts',(-0.12639138516214,8.91322620741042E-5,
0.00934196736194174));
#17069=CARTESIAN_POINT('Ctrl Pts',(-0.126154274972366,-0.0296906128949183,
0.011214877787648));
#17070=CARTESIAN_POINT('Ctrl Pts',(-0.115592373032178,-0.0596151635265703,
0.0130877882133543));
#17071=CARTESIAN_POINT('Ctrl Pts',(-0.0963650578556872,-0.0821635787359664,
0.0149606986390606));
#17072=CARTESIAN_POINT('Ctrl Pts',(-0.0698103971670931,-0.113304978845907,
0.0175473572753932));
#17073=CARTESIAN_POINT('Ctrl Pts',(-0.0267272342632827,-0.130377059081323,
0.0201340159117258));
#17074=CARTESIAN_POINT('Ctrl Pts',(0.0139574509341311,-0.125868770046104,
0.0227206745480584));
#17075=CARTESIAN_POINT('Ctrl Pts',(0.0546421361315456,-0.121360481010885,
0.0253073331843911));
#17076=CARTESIAN_POINT('Ctrl Pts',(0.0929283436225635,-0.0952718227050311,
0.0278939918207237));
#17077=CARTESIAN_POINT('Ctrl Pts',(0.112018291148455,-0.0590635258734944,
0.0304806504570564));
#17078=CARTESIAN_POINT('Ctrl Pts',(0.131108238674346,-0.0228552290419586,
0.033067309093389));
#17079=CARTESIAN_POINT('Ctrl Pts',(0.131001926235112,0.0234727063152593,
0.0356539677297216));
#17080=CARTESIAN_POINT('Ctrl Pts',(0.111741771403992,0.0595891814911641,
0.0382406263660542));
#17081=CARTESIAN_POINT('Ctrl Pts',(0.0924816165728724,0.0957056566670696,
0.0408272850023869));
#17082=CARTESIAN_POINT('Ctrl Pts',(0.0540676193498672,0.121610671661662,
0.0434139436387195));
#17083=CARTESIAN_POINT('Ctrl Pts',(0.0133639835211523,0.125930636937597,
0.0460006022750522));
#17084=CARTESIAN_POINT('Ctrl Pts',(-0.0273396523075625,0.130250602213533,
0.0485872609113848));
#17085=CARTESIAN_POINT('Ctrl Pts',(-0.0703329267419868,0.112985517770812,
0.0511739195477175));
#17086=CARTESIAN_POINT('Ctrl Pts',(-0.0967449447385466,0.0817152626609385,
0.0537605781840501));
#17087=CARTESIAN_POINT('Ctrl Pts',(-0.115741878896724,0.0592240248649833,
0.0556210412433473));
#17088=CARTESIAN_POINT('Ctrl Pts',(-0.126160906676814,0.0294875554882879,
0.0574815043026445));
#17089=CARTESIAN_POINT('Ctrl Pts',(-0.126396145829628,-9.95859796292312E-5,
0.0593419673619417));
#17090=CARTESIAN_POINT('Origin',(0.,0.,0.12));
#17091=CARTESIAN_POINT('',(-0.126529791093031,9.025049583615E-5,0.109341967361942));
#17092=CARTESIAN_POINT('',(-0.126349242904067,8.85860673823967E-5,0.0956580326380584));
#17093=CARTESIAN_POINT('',(-0.12645,1.54856587752183E-17,0.12));
#17094=CARTESIAN_POINT('Ctrl Pts',(-0.126349242904067,8.85860673823967E-5,
0.0956580326380584));
#17095=CARTESIAN_POINT('Ctrl Pts',(-0.126441591528965,0.0135570965972842,
0.0948119253946973));
#17096=CARTESIAN_POINT('Ctrl Pts',(-0.124448136217638,0.0269990101701626,
0.0939658181513361));
#17097=CARTESIAN_POINT('Ctrl Pts',(-0.120249444863787,0.0397126388809939,
0.093119710907975));
#17098=CARTESIAN_POINT('Ctrl Pts',(-0.107413505522824,0.0785798365820317,
0.0905330522716423));
#17099=CARTESIAN_POINT('Ctrl Pts',(-0.0739673525896496,0.110640458354997,
0.0879463936353097));
#17100=CARTESIAN_POINT('Ctrl Pts',(-0.0345920580258737,0.121821308595361,
0.085359734998977));
#17101=CARTESIAN_POINT('Ctrl Pts',(0.00478323653790218,0.133002158835724,
0.0827730763626444));
#17102=CARTESIAN_POINT('Ctrl Pts',(0.0500876727322792,0.123303237543486,
0.0801864177263117));
#17103=CARTESIAN_POINT('Ctrl Pts',(0.0814342209129887,0.0969820390626645,
0.077599759089979));
#17104=CARTESIAN_POINT('Ctrl Pts',(0.112780769093698,0.0706608405818426,
0.0750131004536464));
#17105=CARTESIAN_POINT('Ctrl Pts',(0.13016942926074,0.0277173649124373,
0.0724264418173139));
#17106=CARTESIAN_POINT('Ctrl Pts',(0.12596827751407,-0.0129984006283456,
0.0698397831809812));
#17107=CARTESIAN_POINT('Ctrl Pts',(0.121767125767399,-0.0537141661691284,
0.0672531245446486));
#17108=CARTESIAN_POINT('Ctrl Pts',(0.0959761621070158,-0.0922022215812886,
0.0646664659083159));
#17109=CARTESIAN_POINT('Ctrl Pts',(0.059914723710966,-0.111567668284471,
0.0620798072719833));
#17110=CARTESIAN_POINT('Ctrl Pts',(0.0238532853149157,-0.130933114987654,
0.0594931486356506));
#17111=CARTESIAN_POINT('Ctrl Pts',(-0.0224786278168013,-0.131175952981858,
0.056906489999318));
#17112=CARTESIAN_POINT('Ctrl Pts',(-0.0587401909579078,-0.112190380850839,
0.0543198313629853));
#17113=CARTESIAN_POINT('Ctrl Pts',(-0.0950017540990138,-0.0932048087198191,
0.0517331727266527));
#17114=CARTESIAN_POINT('Ctrl Pts',(-0.12119296724951,-0.0549908264635757,
0.0491465140903201));
#17115=CARTESIAN_POINT('Ctrl Pts',(-0.125823286774378,-0.0143210998620416,
0.0465598554539874));
#17116=CARTESIAN_POINT('Ctrl Pts',(-0.126361397696569,-0.0095946821776348,
0.0462592478486778));
#17117=CARTESIAN_POINT('Ctrl Pts',(-0.12660831057823,-0.00483509759607578,
0.0459586402433681));
#17118=CARTESIAN_POINT('Ctrl Pts',(-0.126575671592806,-7.20628672610732E-5,
0.0456580326380584));
#17119=CARTESIAN_POINT('Ctrl Pts',(-0.126396145829628,-9.95859796292312E-5,
0.0593419673619417));
#17120=CARTESIAN_POINT('Ctrl Pts',(-0.12648796685852,-0.0116483513064931,
0.0600681629389771));
#17121=CARTESIAN_POINT('Ctrl Pts',(-0.125028206814926,-0.0231743653405588,
0.0607943585160125));
#17122=CARTESIAN_POINT('Ctrl Pts',(-0.121921363946098,-0.034237873926493,
0.0615205540930479));
#17123=CARTESIAN_POINT('Ctrl Pts',(-0.110855003598394,-0.0736453296270277,
0.0641072127293806));
#17124=CARTESIAN_POINT('Ctrl Pts',(-0.0788915213442898,-0.107184815251071,
0.0666938713657133));
#17125=CARTESIAN_POINT('Ctrl Pts',(-0.0400617348236378,-0.120133683626334,
0.069280530002046));
#17126=CARTESIAN_POINT('Ctrl Pts',(-0.00123194830298627,-0.133082552001597,
0.0718671886383786));
#17127=CARTESIAN_POINT('Ctrl Pts',(0.0444641424842127,-0.125440803128081,
0.0744538472747112));
#17128=CARTESIAN_POINT('Ctrl Pts',(0.0769682295152699,-0.100563001286921,
0.0770405059110438));
#17129=CARTESIAN_POINT('Ctrl Pts',(0.109472316546327,-0.0756851994457607,
0.0796271645473764));
#17130=CARTESIAN_POINT('Ctrl Pts',(0.128784399821243,-0.0335713446369571,
0.0822138231837091));
#17131=CARTESIAN_POINT('Ctrl Pts',(0.126427276285523,0.00729262199647547,
0.0848004818200417));
#17132=CARTESIAN_POINT('Ctrl Pts',(0.124070152749803,0.0481565886299079,
0.0873871404563744));
#17133=CARTESIAN_POINT('Ctrl Pts',(0.100043822403448,0.0877706670879697,
0.0899737990927071));
#17134=CARTESIAN_POINT('Ctrl Pts',(0.0648947831756147,0.108746049780439,
0.0925604577290397));
#17135=CARTESIAN_POINT('Ctrl Pts',(0.0297457439477817,0.129721432472907,
0.0951471163653723));
#17136=CARTESIAN_POINT('Ctrl Pts',(-0.0165260041615291,0.132058119399784,
0.0977337750017049));
#17137=CARTESIAN_POINT('Ctrl Pts',(-0.0536093211433369,0.114730442741844,
0.100320433638038));
#17138=CARTESIAN_POINT('Ctrl Pts',(-0.0906926381251451,0.0974027660839045,
0.10290709227437));
#17139=CARTESIAN_POINT('Ctrl Pts',(-0.11858752397945,0.0604107258411485,
0.105493750910703));
#17140=CARTESIAN_POINT('Ctrl Pts',(-0.12504939731921,0.0199921027543164,
0.108080409547035));
#17141=CARTESIAN_POINT('Ctrl Pts',(-0.126099919499473,0.0134211506765118,
0.108500928818671));
#17142=CARTESIAN_POINT('Ctrl Pts',(-0.126583971845017,0.00675963476331471,
0.108921448090306));
#17143=CARTESIAN_POINT('Ctrl Pts',(-0.126529791093031,9.025049583615E-5,
0.109341967361942));
#17144=CARTESIAN_POINT('Origin',(0.,0.,0.12));
#17145=CARTESIAN_POINT('',(-0.126296536029262,-6.10717992316628E-5,0.159341967361942));
#17146=CARTESIAN_POINT('',(-0.126453631260982,-0.000102348163238207,0.145658032638058));
#17147=CARTESIAN_POINT('',(-0.12645,1.54856587752183E-17,0.12));
#17148=CARTESIAN_POINT('Ctrl Pts',(-0.126453631260982,-0.000102348163238207,
0.145658032638058));
#17149=CARTESIAN_POINT('Ctrl Pts',(-0.126183364177612,0.031552920325249,
0.143665210546026));
#17150=CARTESIAN_POINT('Ctrl Pts',(-0.114073771100105,0.0633928690595716,
0.141672388453994));
#17151=CARTESIAN_POINT('Ctrl Pts',(-0.0925489356314354,0.0864391430514358,
0.139679566361962));
#17152=CARTESIAN_POINT('Ctrl Pts',(-0.0646099631645552,0.116352924063146,
0.13709290772563));
#17153=CARTESIAN_POINT('Ctrl Pts',(-0.0208084524006029,0.131451366650306,
0.134506249089297));
#17154=CARTESIAN_POINT('Ctrl Pts',(0.0196287675426836,0.125106932552633,
0.131919590452964));
#17155=CARTESIAN_POINT('Ctrl Pts',(0.0600659874859703,0.11876249845496,
0.129332931816632));
#17156=CARTESIAN_POINT('Ctrl Pts',(0.097138916608591,0.0909751876724545,
0.126746273180299));
#17157=CARTESIAN_POINT('Ctrl Pts',(0.114574233156503,0.0539423598350403,
0.124159614543967));
#17158=CARTESIAN_POINT('Ctrl Pts',(0.132009549704415,0.0169095319976262,
0.121572955907634));
#17159=CARTESIAN_POINT('Ctrl Pts',(0.129807253677619,-0.0293688128946969,
0.118986297271301));
#17160=CARTESIAN_POINT('Ctrl Pts',(0.108934072954415,-0.0645786240759305,
0.116399638634969));
#17161=CARTESIAN_POINT('Ctrl Pts',(0.0880608922312115,-0.099788435257164,
0.113812979998636));
#17162=CARTESIAN_POINT('Ctrl Pts',(0.0485168268116012,-0.123929712727308,
0.111226321362303));
#17163=CARTESIAN_POINT('Ctrl Pts',(0.00765986125275547,-0.126405537442516,
0.108639662725971));
#17164=CARTESIAN_POINT('Ctrl Pts',(-0.0331971043060904,-0.128881362157723,
0.106053004089638));
#17165=CARTESIAN_POINT('Ctrl Pts',(-0.0753669700041717,-0.109691734117994,
0.103466345453305));
#17166=CARTESIAN_POINT('Ctrl Pts',(-0.100339039978837,-0.0772600332835736,
0.100879686816973));
#17167=CARTESIAN_POINT('Ctrl Pts',(-0.117142637704978,-0.0554368822612891,
0.0991391354240014));
#17168=CARTESIAN_POINT('Ctrl Pts',(-0.126159269908366,-0.0276178718881664,
0.0973985840310299));
#17169=CARTESIAN_POINT('Ctrl Pts',(-0.126349242904067,8.85860673823967E-5,
0.0956580326380584));
#17170=CARTESIAN_POINT('Ctrl Pts',(-0.126529791093031,9.025049583615E-5,
0.109341967361942));
#17171=CARTESIAN_POINT('Ctrl Pts',(-0.126250700293628,-0.0342644551610371,
0.111508106726639));
#17172=CARTESIAN_POINT('Ctrl Pts',(-0.111690189779818,-0.0688279388928191,
0.113674246091336));
#17173=CARTESIAN_POINT('Ctrl Pts',(-0.0867076257192948,-0.092297473337895,
0.115840385456033));
#17174=CARTESIAN_POINT('Ctrl Pts',(-0.0568751199544048,-0.120323220412367,
0.118427044092366));
#17175=CARTESIAN_POINT('Ctrl Pts',(-0.0121812475994092,-0.132529508630403,
0.121013702728699));
#17176=CARTESIAN_POINT('Ctrl Pts',(0.0277554439013372,-0.123558363290506,
0.123600361365031));
#17177=CARTESIAN_POINT('Ctrl Pts',(0.0676921354020838,-0.114587217950609,
0.126187020001364));
#17178=CARTESIAN_POINT('Ctrl Pts',(0.102871646048582,-0.0844386390527785,
0.128773678637697));
#17179=CARTESIAN_POINT('Ctrl Pts',(0.117851793294146,-0.0463464242807743,
0.131360337274029));
#17180=CARTESIAN_POINT('Ctrl Pts',(0.13283194053971,-0.00825420950877041,
0.133946995910362));
#17181=CARTESIAN_POINT('Ctrl Pts',(0.127612724384341,0.0377816411374068,
0.136533654546694));
#17182=CARTESIAN_POINT('Ctrl Pts',(0.104485135941302,0.0715534408109559,
0.139120313183027));
#17183=CARTESIAN_POINT('Ctrl Pts',(0.0813575474982633,0.105325240484505,
0.14170697181936));
#17184=CARTESIAN_POINT('Ctrl Pts',(0.0403215867675544,0.126832989185426,
0.144293630455692));
#17185=CARTESIAN_POINT('Ctrl Pts',(-0.000609841963000384,0.126635909896556,
0.146880289092025));
#17186=CARTESIAN_POINT('Ctrl Pts',(-0.0415412706935549,0.126438830607686,
0.149466947728358));
#17187=CARTESIAN_POINT('Ctrl Pts',(-0.0823681674239554,0.104536923329025,
0.15205360636469));
#17188=CARTESIAN_POINT('Ctrl Pts',(-0.10516942503222,0.0705438627883669,
0.154640265001023));
#17189=CARTESIAN_POINT('Ctrl Pts',(-0.118984510025511,0.0499477610899654,
0.156207499121329));
#17190=CARTESIAN_POINT('Ctrl Pts',(-0.126182304652747,0.0249129445447297,
0.157774733241635));
#17191=CARTESIAN_POINT('Ctrl Pts',(-0.126296536029262,-6.10717992316628E-5,
0.159341967361942));
#17192=CARTESIAN_POINT('Origin',(0.,0.,0.12));
#17193=CARTESIAN_POINT('',(-0.126625441102054,2.7778768752873E-5,0.209341967361942));
#17194=CARTESIAN_POINT('',(-0.126471935391749,0.000101176582396995,0.195658032638058));
#17195=CARTESIAN_POINT('',(-0.12645,1.54856587752183E-17,0.12));
#17196=CARTESIAN_POINT('',(0.0958116152722397,0.0825211298936481,0.24));
#17197=CARTESIAN_POINT('Ctrl Pts',(-0.126625441102054,2.7778768752873E-5,
0.209341967361942));
#17198=CARTESIAN_POINT('Ctrl Pts',(-0.126482885932031,-0.0388928622545336,
0.21180133566563));
#17199=CARTESIAN_POINT('Ctrl Pts',(-0.107125339127294,-0.077921419747323,
0.214260703969318));
#17200=CARTESIAN_POINT('Ctrl Pts',(-0.0759952538809665,-0.101287130411732,
0.216720072273006));
#17201=CARTESIAN_POINT('Ctrl Pts',(-0.0432539585932993,-0.12586218783339,
0.219306730909339));
#17202=CARTESIAN_POINT('Ctrl Pts',(0.0025100419330305,-0.133111106253138,
0.221893389545672));
#17203=CARTESIAN_POINT('Ctrl Pts',(0.0412155518054008,-0.119764891216682,
0.224480048182004));
#17204=CARTESIAN_POINT('Ctrl Pts',(0.0799210616777711,-0.106418676180227,
0.227066706818337));
#17205=CARTESIAN_POINT('Ctrl Pts',(0.111568080896182,-0.072477327687567,
0.229653365454669));
#17206=CARTESIAN_POINT('Ctrl Pts',(0.122246574267713,-0.0330282462555153,
0.232240024091002));
#17207=CARTESIAN_POINT('Ctrl Pts',(0.132925067639245,0.00642083517653631,
0.234826682727335));
#17208=CARTESIAN_POINT('Ctrl Pts',(0.122635035163896,0.0513776495479799,
0.237413341363667));
#17209=CARTESIAN_POINT('Ctrl Pts',(0.0958116152722397,0.0825211298936481,
0.24));
#17210=CARTESIAN_POINT('',(-0.0959791030802601,0.0826138105732953,0.24));
#17211=CARTESIAN_POINT('Origin',(0.,0.,0.24));
#17212=CARTESIAN_POINT('Ctrl Pts',(-0.0959791030802601,0.0826138105732953,
0.24));
#17213=CARTESIAN_POINT('Ctrl Pts',(-0.0710417758635208,0.111296717646776,
0.237599759089979));
#17214=CARTESIAN_POINT('Ctrl Pts',(-0.0322351762885183,0.128218895525122,
0.235199518179958));
#17215=CARTESIAN_POINT('Ctrl Pts',(0.00571352152256588,0.126497857083363,
0.232799277269937));
#17216=CARTESIAN_POINT('Ctrl Pts',(0.0466095526337785,0.124643152028446,
0.230212618633605));
#17217=CARTESIAN_POINT('Ctrl Pts',(0.0865092470399708,0.101136876245298,
0.227625959997272));
#17218=CARTESIAN_POINT('Ctrl Pts',(0.107920636628548,0.0662586835305903,
0.225039301360939));
#17219=CARTESIAN_POINT('Ctrl Pts',(0.129332026217125,0.0313804908158828,
0.222452642724607));
#17220=CARTESIAN_POINT('Ctrl Pts',(0.132255110988087,-0.014869618830384,
0.219865984088274));
#17221=CARTESIAN_POINT('Ctrl Pts',(0.115395215428634,-0.0521699181865619,
0.217279325451942));
#17222=CARTESIAN_POINT('Ctrl Pts',(0.0985353198691812,-0.0894702175427398,
0.214692666815609));
#17223=CARTESIAN_POINT('Ctrl Pts',(0.0618924439793129,-0.117820706608829,
0.212106008179276));
#17224=CARTESIAN_POINT('Ctrl Pts',(0.0215571925812854,-0.12478734248304,
0.209519349542944));
#17225=CARTESIAN_POINT('Ctrl Pts',(-0.0187780588167422,-0.13175397835725,
0.206932690906611));
#17226=CARTESIAN_POINT('Ctrl Pts',(-0.0628056857229291,-0.117336761039583,
0.204346032270278));
#17227=CARTESIAN_POINT('Ctrl Pts',(-0.0912027768750998,-0.0878586653637446,
0.201759373633946));
#17228=CARTESIAN_POINT('Ctrl Pts',(-0.113530209130371,-0.0646812849521466,
0.199725593301983));
#17229=CARTESIAN_POINT('Ctrl Pts',(-0.126194825294183,-0.0321932513395888,
0.197691812970021));
#17230=CARTESIAN_POINT('Ctrl Pts',(-0.126471935391749,0.000101176582396995,
0.195658032638058));
#17231=CARTESIAN_POINT('Origin',(0.,0.,0.350421172358873));
#17232=CARTESIAN_POINT('',(-0.154453350152392,-8.79343647196378E-5,0.0295788276411275));
#17233=CARTESIAN_POINT('',(-0.15422847552802,0.000108763211052777,0.025421172358873));
#17234=CARTESIAN_POINT('',(-0.1543,-1.01731279388251E-15,0.350421172358873));
#17235=CARTESIAN_POINT('',(0.15408394018464,-0.00816268198427004,0.));
#17236=CARTESIAN_POINT('Ctrl Pts',(-0.15422847552802,0.000108763211052763,
0.025421172358873));
#17237=CARTESIAN_POINT('Ctrl Pts',(-0.154338737393477,0.0139570514561378,
0.0247074241482466));
#17238=CARTESIAN_POINT('Ctrl Pts',(-0.146387882101843,0.0778735560251454,
0.0214070173012875));
#17239=CARTESIAN_POINT('Ctrl Pts',(-0.0581466660421577,0.171532975008042,
0.0155199518179959));
#17240=CARTESIAN_POINT('Ctrl Pts',(0.109502662757235,0.144085240745689,
0.00775997590899784));
#17241=CARTESIAN_POINT('Ctrl Pts',(0.156737212705124,0.0419221657566679,
0.00258665863633264));
#17242=CARTESIAN_POINT('Ctrl Pts',(0.15408394018464,-0.00816268198427004,
0.));
#17243=CARTESIAN_POINT('',(0.129620323775263,-0.0841289546921688,3.62607491890453E-17));
#17244=CARTESIAN_POINT('Origin',(0.,0.,0.));
#17245=CARTESIAN_POINT('Ctrl Pts',(-0.154453350152392,-8.7934364719636E-5,
0.0295788276411275));
#17246=CARTESIAN_POINT('Ctrl Pts',(-0.154150470777978,0.0441115087317509,
0.0272927766101045));
#17247=CARTESIAN_POINT('Ctrl Pts',(-0.111454882743928,0.138841433785012,
0.0224200669427489));
#17248=CARTESIAN_POINT('Ctrl Pts',(0.0476444145610997,0.174632482457551,
0.0149606986390605));
#17249=CARTESIAN_POINT('Ctrl Pts',(0.168251138196633,0.0613688951001999,
0.0073871404563744));
#17250=CARTESIAN_POINT('Ctrl Pts',(0.154676764047789,-0.0451013867871701,
0.00240024091002087));
#17251=CARTESIAN_POINT('Ctrl Pts',(0.129620323775263,-0.0841289546921688,
1.57209315010398E-17));
#17252=CARTESIAN_POINT('Origin',(0.,0.,0.350421172358873));
#17253=CARTESIAN_POINT('',(-0.154177051641736,0.000108096719625833,0.0795788276411275));
#17254=CARTESIAN_POINT('',(-0.154234284709463,-0.000121519309271207,0.075421172358873));
#17255=CARTESIAN_POINT('',(-0.1543,-1.01731279388251E-15,0.350421172358873));
#17256=CARTESIAN_POINT('Ctrl Pts',(-0.154234284709463,-0.000121519309271208,
0.0754211723588731));
#17257=CARTESIAN_POINT('Ctrl Pts',(-0.153947235272697,0.0359820467524117,
0.0735607092995758));
#17258=CARTESIAN_POINT('Ctrl Pts',(-0.123557126730793,0.122717061869437,
0.0691135876039459));
#17259=CARTESIAN_POINT('Ctrl Pts',(0.0191012565771036,0.180005302104073,
0.0620798072719832));
#17260=CARTESIAN_POINT('Ctrl Pts',(0.159724738700703,0.0851738948996701,
0.0543198313629854));
#17261=CARTESIAN_POINT('Ctrl Pts',(0.160113920417758,-0.0844204212478698,
0.0465598554539874));
#17262=CARTESIAN_POINT('Ctrl Pts',(0.0199582426985643,-0.179924098035372,
0.0387998795449896));
#17263=CARTESIAN_POINT('Ctrl Pts',(-0.123251388539896,-0.123176028715441,
0.0317536518466181));
#17264=CARTESIAN_POINT('Ctrl Pts',(-0.153939142967466,-0.0362298265692857,
0.0272940827845792));
#17265=CARTESIAN_POINT('Ctrl Pts',(-0.15422847552802,0.000108763211052763,
0.025421172358873));
#17266=CARTESIAN_POINT('Ctrl Pts',(-0.154177051641736,0.000108096719625859,
0.0795788276411275));
#17267=CARTESIAN_POINT('Ctrl Pts',(-0.154289739603949,0.0165429814548096,
0.0787327203977663));
#17268=CARTESIAN_POINT('Ctrl Pts',(-0.144420757340354,0.0830897487115299,
0.0752999545180725));
#17269=CARTESIAN_POINT('Ctrl Pts',(-0.0494457976037486,0.174130301808973,
0.0692805300020459));
#17270=CARTESIAN_POINT('Ctrl Pts',(0.11640175885633,0.13862511662766,0.061520554093048));
#17271=CARTESIAN_POINT('Ctrl Pts',(0.18005704388064,-0.0185795878987759,
0.0537605781840501));
#17272=CARTESIAN_POINT('Ctrl Pts',(0.0856431484406112,-0.159474177462153,
0.0460006022750521));
#17273=CARTESIAN_POINT('Ctrl Pts',(-0.0839657292871194,-0.160363143120653,
0.0382406263660544));
#17274=CARTESIAN_POINT('Ctrl Pts',(-0.151599316432495,-0.0616831513139142,
0.0327667014880793));
#17275=CARTESIAN_POINT('Ctrl Pts',(-0.154493177716258,-0.00590000442131094,
0.0298794352464371));
#17276=CARTESIAN_POINT('Ctrl Pts',(-0.154453350152392,-8.7934364719636E-5,
0.0295788276411275));
#17277=CARTESIAN_POINT('Origin',(0.,0.,0.350421172358873));
#17278=CARTESIAN_POINT('',(-0.154304431028624,-0.000124889850439479,0.129578827641127));
#17279=CARTESIAN_POINT('',(-0.154397364694779,0.000110127730384366,0.125421172358873));
#17280=CARTESIAN_POINT('',(-0.1543,-1.01731279388251E-15,0.350421172358873));
#17281=CARTESIAN_POINT('Ctrl Pts',(-0.154397364694779,0.000110127730384357,
0.125421172358873));
#17282=CARTESIAN_POINT('Ctrl Pts',(-0.154463478494948,0.00824841157753406,
0.125000653087238));
#17283=CARTESIAN_POINT('Ctrl Pts',(-0.150239588102603,0.0663774823757793,
0.121993475179269));
#17284=CARTESIAN_POINT('Ctrl Pts',(-0.0766286530280003,0.163994611436961,
0.116399638634969));
#17285=CARTESIAN_POINT('Ctrl Pts',(0.0927599764682439,0.155440618724813,
0.108639662725971));
#17286=CARTESIAN_POINT('Ctrl Pts',(0.180714016146597,0.0104239566588842,
0.100879686816973));
#17287=CARTESIAN_POINT('Ctrl Pts',(0.11001758793024,-0.143743725357685,
0.093119710907975));
#17288=CARTESIAN_POINT('Ctrl Pts',(-0.0572637123892103,-0.171718146500831,
0.0853597349989769));
#17289=CARTESIAN_POINT('Ctrl Pts',(-0.146220320052713,-0.0783754111826042,
0.0794602221492764));
#17290=CARTESIAN_POINT('Ctrl Pts',(-0.154346328875204,-0.0142138442593302,
0.0761473679359084));
#17291=CARTESIAN_POINT('Ctrl Pts',(-0.154234284709463,-0.000121519309271208,
0.0754211723588731));
#17292=CARTESIAN_POINT('Ctrl Pts',(-0.154304431028624,-0.000124889850439474,
0.129578827641127));
#17293=CARTESIAN_POINT('Ctrl Pts',(-0.153974638929265,0.0385022981904757,
0.127586005549095));
#17294=CARTESIAN_POINT('Ctrl Pts',(-0.120018027207353,0.127784966030512,
0.123006524820731));
#17295=CARTESIAN_POINT('Ctrl Pts',(0.0280571680938306,0.178826694862324,
0.115840385456033));
#17296=CARTESIAN_POINT('Ctrl Pts',(0.163771354656592,0.0771047007047774,
0.108080409547035));
#17297=CARTESIAN_POINT('Ctrl Pts',(0.155709331479018,-0.0923080778690166,
0.100320433638038));
#17298=CARTESIAN_POINT('Ctrl Pts',(0.0109489686262093,-0.180682908560435,
0.0925604577290397));
#17299=CARTESIAN_POINT('Ctrl Pts',(-0.126591758993125,-0.118094248159534,
0.0856465890634029));
#17300=CARTESIAN_POINT('Ctrl Pts',(-0.153945238013925,-0.0337005743957639,
0.0813193790340989));
#17301=CARTESIAN_POINT('Ctrl Pts',(-0.154177051641736,0.000108096719625859,
0.0795788276411275));
#17302=CARTESIAN_POINT('Origin',(0.,0.,0.350421172358873));
#17303=CARTESIAN_POINT('',(-0.154326766555531,0.000123460234585843,0.179578827641127));
#17304=CARTESIAN_POINT('',(-0.154112736333057,-7.45225671948511E-5,0.175421172358873));
#17305=CARTESIAN_POINT('',(-0.1543,-1.01731279388251E-15,0.350421172358873));
#17306=CARTESIAN_POINT('Ctrl Pts',(-0.154112736333057,-7.45225671948471E-5,
0.175421172358873));
#17307=CARTESIAN_POINT('Ctrl Pts',(-0.153973346049181,0.0303998999070902,
0.173853938238567));
#17308=CARTESIAN_POINT('Ctrl Pts',(-0.130694151755309,0.111367805862998,
0.169700045481928));
#17309=CARTESIAN_POINT('Ctrl Pts',(-0.000871711368246156,0.181012066871201,
0.162959494088956));
#17310=CARTESIAN_POINT('Ctrl Pts',(0.149350085565286,0.102277888352765,
0.155199518179958));
#17311=CARTESIAN_POINT('Ctrl Pts',(0.168456255263351,-0.0662471829332422,
0.14743954227096));
#17312=CARTESIAN_POINT('Ctrl Pts',(0.0396733728729688,-0.17661315503135,
0.139679566361963));
#17313=CARTESIAN_POINT('Ctrl Pts',(-0.115072782317819,-0.134350623919955,
0.1323401097246));
#17314=CARTESIAN_POINT('Ctrl Pts',(-0.154056805498669,-0.041811035439686,
0.12758731172357));
#17315=CARTESIAN_POINT('Ctrl Pts',(-0.154397364694779,0.000110127730384357,
0.125421172358873));
#17316=CARTESIAN_POINT('Ctrl Pts',(-0.154326766555531,0.000123460234585825,
0.179578827641127));
#17317=CARTESIAN_POINT('Ctrl Pts',(-0.154418689716183,0.0108361910665024,
0.179025949336757));
#17318=CARTESIAN_POINT('Ctrl Pts',(-0.148597337680631,0.071569631208062,
0.175886412396054));
#17319=CARTESIAN_POINT('Ctrl Pts',(-0.0683530255288039,0.167611467503216,
0.170160216819019));
#17320=CARTESIAN_POINT('Ctrl Pts',(0.100397202365132,0.150621028353064,
0.162400240910021));
#17321=CARTESIAN_POINT('Ctrl Pts',(0.18100910679194,0.00139719974911195,
0.154640265001023));
#17322=CARTESIAN_POINT('Ctrl Pts',(0.102711092909207,-0.149052183789333,
0.146880289092025));
#17323=CARTESIAN_POINT('Ctrl Pts',(-0.0657574679958034,-0.168648048308422,
0.139120313183027));
#17324=CARTESIAN_POINT('Ctrl Pts',(-0.148058381688037,-0.0731761882111772,
0.133353159366061));
#17325=CARTESIAN_POINT('Ctrl Pts',(-0.154402705029802,-0.0116353181791797,
0.130172664185428));
#17326=CARTESIAN_POINT('Ctrl Pts',(-0.154304431028624,-0.000124889850439474,
0.129578827641127));
#17327=CARTESIAN_POINT('Origin',(0.,0.,0.350421172358873));
#17328=CARTESIAN_POINT('',(-0.154128406284035,-0.000157308197905263,0.229578827641128));
#17329=CARTESIAN_POINT('',(-0.154514081154978,3.38969080117728E-5,0.225421172358873));
#17330=CARTESIAN_POINT('',(-0.1543,-1.01731279388251E-15,0.350421172358873));
#17331=CARTESIAN_POINT('',(-0.0398513841857245,-0.149064942821851,0.24));
#17332=CARTESIAN_POINT('Ctrl Pts',(-0.0398513841857245,-0.149064942821851,
0.24));
#17333=CARTESIAN_POINT('Ctrl Pts',(-0.0883048112969314,-0.136111285829332,
0.237413341363667));
#17334=CARTESIAN_POINT('Ctrl Pts',(-0.143745772087175,-0.0847488633265083,
0.233939617244043));
#17335=CARTESIAN_POINT('Ctrl Pts',(-0.154234229255939,-0.017399338864059,
0.230465893124419));
#17336=CARTESIAN_POINT('Ctrl Pts',(-0.154128406284035,-0.00015730819790527,
0.229578827641128));
#17337=CARTESIAN_POINT('',(0.0399565498027962,-0.149273502906638,0.24));
#17338=CARTESIAN_POINT('Origin',(0.,0.,0.24));
#17339=CARTESIAN_POINT('Ctrl Pts',(0.0399565498027963,-0.149273502906638,
0.24));
#17340=CARTESIAN_POINT('Ctrl Pts',(-0.00490373130458673,-0.161043406468747,
0.237599759089979));
#17341=CARTESIAN_POINT('Ctrl Pts',(-0.107666111297752,-0.141562671532916,
0.23274014987627));
#17342=CARTESIAN_POINT('Ctrl Pts',(-0.154340128899266,-0.0474588267763927,
0.227880540662561));
#17343=CARTESIAN_POINT('Ctrl Pts',(-0.154514081154978,3.3896908011755E-5,
0.225421172358873));
#17344=CARTESIAN_POINT('Origin',(0.,0.,0.350421172358873));
#17345=CARTESIAN_POINT('Ctrl Pts',(-0.154514081154978,3.3896908011755E-5,
0.225421172358873));
#17346=CARTESIAN_POINT('Ctrl Pts',(-0.154523084458981,0.00249199339844659,
0.225293882026228));
#17347=CARTESIAN_POINT('Ctrl Pts',(-0.153375868586475,0.0548933889046004,
0.222579933057251));
#17348=CARTESIAN_POINT('Ctrl Pts',(-0.0942515706791253,0.154556313135293,
0.217279325451942));
#17349=CARTESIAN_POINT('Ctrl Pts',(0.0750450248431312,0.164716481511431,
0.209519349542944));
#17350=CARTESIAN_POINT('Ctrl Pts',(0.178461260043253,0.0303012077178856,
0.201759373633945));
#17351=CARTESIAN_POINT('Ctrl Pts',(0.125203781387627,-0.130731709675357,
0.193999397724948));
#17352=CARTESIAN_POINT('Ctrl Pts',(-0.0379704533096903,-0.17698585337688,
0.18623942181595));
#17353=CARTESIAN_POINT('Ctrl Pts',(-0.141587477595567,-0.0899051669249145,
0.180046680027258));
#17354=CARTESIAN_POINT('Ctrl Pts',(-0.154203404262525,-0.019896942829432,
0.176440596874899));
#17355=CARTESIAN_POINT('Ctrl Pts',(-0.154112736333057,-7.45225671948471E-5,
0.175421172358873));
#17356=CARTESIAN_POINT('Ctrl Pts',(-0.154128406284035,-0.00015730819790527,
0.229578827641128));
#17357=CARTESIAN_POINT('Ctrl Pts',(-0.153925652370292,0.0328779499839183,
0.227879234488086));
#17358=CARTESIAN_POINT('Ctrl Pts',(-0.127638532780061,0.116591914860373,
0.223592982698713));
#17359=CARTESIAN_POINT('Ctrl Pts',(0.00818767200092134,0.180778621679153,
0.216720072273006));
#17360=CARTESIAN_POINT('Ctrl Pts',(0.154249898498561,0.0947283641859207,
0.208960096364008));
#17361=CARTESIAN_POINT('Ctrl Pts',(0.164950538597243,-0.0745810526211722,
0.201200120455011));
#17362=CARTESIAN_POINT('Ctrl Pts',(0.0308106631569891,-0.178364693496558,
0.193440144546012));
#17363=CARTESIAN_POINT('Ctrl Pts',(-0.118879635670858,-0.129347344159377,
0.186233046941385));
#17364=CARTESIAN_POINT('Ctrl Pts',(-0.153988624301243,-0.0392836590090855,
0.18161260797309));
#17365=CARTESIAN_POINT('Ctrl Pts',(-0.154326766555531,0.000123460234585825,
0.179578827641127));
#17366=CARTESIAN_POINT('Ctrl Pts',(0.0958116152722397,0.0825211298936481,
0.24));
#17367=CARTESIAN_POINT('Ctrl Pts',(0.122635035163896,0.0513776495479799,
0.237413341363667));
#17368=CARTESIAN_POINT('Ctrl Pts',(0.143215100114593,-0.0385359791949074,
0.232240024091002));
#17369=CARTESIAN_POINT('Ctrl Pts',(0.0482740424593604,-0.140360024672886,
0.224480048182004));
#17370=CARTESIAN_POINT('Ctrl Pts',(-0.0890179591196291,-0.118613269413641,
0.216720072273006));
#17371=CARTESIAN_POINT('Ctrl Pts',(-0.148173729266643,0.00709031985706173,
0.208960096364008));
#17372=CARTESIAN_POINT('Ctrl Pts',(-0.0772398646297824,0.126660050524678,
0.20120012045501));
#17373=CARTESIAN_POINT('Ctrl Pts',(0.0614999571705377,0.134986384232796,
0.193440144546013));
#17374=CARTESIAN_POINT('Ctrl Pts',(0.146250332679645,0.0248320655601208,
0.185680168637014));
#17375=CARTESIAN_POINT('Ctrl Pts',(0.102605431992647,-0.107135610424167,
0.177920192728017));
#17376=CARTESIAN_POINT('Ctrl Pts',(-0.0311170694815965,-0.145041225920327,
0.170160216819019));
#17377=CARTESIAN_POINT('Ctrl Pts',(-0.137521919612742,-0.0556176253575994,
0.162400240910021));
#17378=CARTESIAN_POINT('Ctrl Pts',(-0.123195064154356,0.0826350160503635,
0.154640265001023));
#17379=CARTESIAN_POINT('Ctrl Pts',(-0.000714373963154436,0.148340737886347,
0.146880289092025));
#17380=CARTESIAN_POINT('Ctrl Pts',(0.122393508228972,0.0838174917835845,
0.139120313183027));
#17381=CARTESIAN_POINT('Ctrl Pts',(0.138051156695079,-0.0542900601549481,
0.131360337274029));
#17382=CARTESIAN_POINT('Ctrl Pts',(0.032512624755586,-0.14473579684844,
0.123600361365031));
#17383=CARTESIAN_POINT('Ctrl Pts',(-0.101568992309399,-0.108116932194331,
0.115840385456033));
#17384=CARTESIAN_POINT('Ctrl Pts',(-0.146482409833755,0.0234186855983926,
0.108080409547036));
#17385=CARTESIAN_POINT('Ctrl Pts',(-0.0627977522708403,0.13439480632666,
0.100320433638038));
#17386=CARTESIAN_POINT('Ctrl Pts',(0.076017492057093,0.127384745546031,
0.0925604577290397));
#17387=CARTESIAN_POINT('Ctrl Pts',(0.148096483096158,0.00854251017184644,
0.0848004818200417));
#17388=CARTESIAN_POINT('Ctrl Pts',(0.0901602332714121,-0.117799054254564,
0.0770405059110438));
#17389=CARTESIAN_POINT('Ctrl Pts',(-0.0469280390901857,-0.140724300875114,
0.069280530002046));
#17390=CARTESIAN_POINT('Ctrl Pts',(-0.142818485852497,-0.0401058440029853,
0.0615205540930479));
#17391=CARTESIAN_POINT('Ctrl Pts',(-0.113326201176411,0.0957204333280909,
0.0537605781840501));
#17392=CARTESIAN_POINT('Ctrl Pts',(0.0156536221268617,0.147515686656254,
0.0460006022750521));
#17393=CARTESIAN_POINT('Ctrl Pts',(0.130895613795878,0.0698006416724775,
0.0382406263660543));
#17394=CARTESIAN_POINT('Ctrl Pts',(0.13121455111358,-0.0691831643991777,
0.0304806504570563));
#17395=CARTESIAN_POINT('Ctrl Pts',(0.0163559286405278,-0.147449139316739,
0.0227206745480584));
#17396=CARTESIAN_POINT('Ctrl Pts',(-0.112893560070904,-0.0962328986104914,
0.0149606986390606));
#17397=CARTESIAN_POINT('Ctrl Pts',(-0.142972035491037,0.0393992613429074,
0.00720072273006258));
#17398=CARTESIAN_POINT('Ctrl Pts',(-0.0476516261894416,0.140572551456688,
-0.000559253178935252));
#17399=CARTESIAN_POINT('Ctrl Pts',(0.0897382482543901,0.118078928660352,
-0.00831922908793326));
#17400=CARTESIAN_POINT('Ctrl Pts',(0.128447313976429,0.0343555272840613,
-0.0134925463605985));
#17401=CARTESIAN_POINT('Ctrl Pts',(0.126272937371016,-0.00668937872268922,
-0.0160792049969311));
#17402=CARTESIAN_POINT('Ctrl Pts',(0.102845629995666,0.0885794229410663,
0.245359734998977));
#17403=CARTESIAN_POINT('Ctrl Pts',(0.13163829265517,0.0551495423644061,
0.242773076362644));
#17404=CARTESIAN_POINT('Ctrl Pts',(0.153729244145676,-0.0413651001137901,
0.237599759089979));
#17405=CARTESIAN_POINT('Ctrl Pts',(0.0518180837997932,-0.150664563191773,
0.229839783180981));
#17406=CARTESIAN_POINT('Ctrl Pts',(-0.0955532172229155,-0.127321268762976,
0.222079807271983));
#17407=CARTESIAN_POINT('Ctrl Pts',(-0.159051911315084,0.00761085605850937,
0.214319831362985));
#17408=CARTESIAN_POINT('Ctrl Pts',(-0.0829104333128967,0.135958804728216,
0.206559855453988));
#17409=CARTESIAN_POINT('Ctrl Pts',(0.0660149797280689,0.144896416659008,
0.19879987954499));
#17410=CARTESIAN_POINT('Ctrl Pts',(0.156987308467515,0.0266551129460425,
0.191039903635992));
#17411=CARTESIAN_POINT('Ctrl Pts',(0.110138215124307,-0.11500097684123,
0.183279927726994));
#17412=CARTESIAN_POINT('Ctrl Pts',(-0.0334015307576278,-0.155689435072511,
0.175519951817996));
#17413=CARTESIAN_POINT('Ctrl Pts',(-0.147618098500879,-0.0597007962188336,
0.167759975908998));
#17414=CARTESIAN_POINT('Ctrl Pts',(-0.13223943620312,0.0887016700559064,
0.16));
#17415=CARTESIAN_POINT('Ctrl Pts',(-0.000766819764851659,0.159231180881298,
0.152240024091002));
#17416=CARTESIAN_POINT('Ctrl Pts',(0.131379034007743,0.0899709573066447,
0.144480048182004));
#17417=CARTESIAN_POINT('Ctrl Pts',(0.14818618955117,-0.0582757677477129,
0.136720072273006));
#17418=CARTESIAN_POINT('Ctrl Pts',(0.0348995407947136,-0.15536158290941,
0.128960096364009));
#17419=CARTESIAN_POINT('Ctrl Pts',(-0.109025685167754,-0.116054342400242,
0.12120012045501));
#17420=CARTESIAN_POINT('Ctrl Pts',(-0.157236423577976,0.0251379696208395,
0.113440144546013));
#17421=CARTESIAN_POINT('Ctrl Pts',(-0.0674080525232269,0.144261408030094,
0.105680168637014));
#17422=CARTESIAN_POINT('Ctrl Pts',(0.0815983201941432,0.136736703272292,
0.0979201927280168));
#17423=CARTESIAN_POINT('Ctrl Pts',(0.158968994112971,0.00916965900085902,
0.0901602168190187));
#17424=CARTESIAN_POINT('Ctrl Pts',(0.0967793514910216,-0.126447277955604,
0.0824002409100209));
#17425=CARTESIAN_POINT('Ctrl Pts',(-0.0503732635231939,-0.151055582750353,
0.0746402650010229));
#17426=CARTESIAN_POINT('Ctrl Pts',(-0.15330351242688,-0.0430502166284845,
0.066880289092025));
#17427=CARTESIAN_POINT('Ctrl Pts',(-0.121646050135849,0.102747753924341,
0.0591203131830272));
#17428=CARTESIAN_POINT('Ctrl Pts',(0.0168028336102756,0.158345558472194,
0.0513603372740292));
#17429=CARTESIAN_POINT('Ctrl Pts',(0.140505322097486,0.074925059414875,
0.0436003613650313));
#17430=CARTESIAN_POINT('Ctrl Pts',(0.140847674214973,-0.0742622500154084,
0.0358403854560334));
#17431=CARTESIAN_POINT('Ctrl Pts',(0.0175566999932067,-0.158274125556283,
0.0280804095470355));
#17432=CARTESIAN_POINT('Ctrl Pts',(-0.121181646661057,-0.103297841872129,
0.0203204336380376));
#17433=CARTESIAN_POINT('Ctrl Pts',(-0.153468334920127,0.0422917601656304,
0.0125604577290396));
#17434=CARTESIAN_POINT('Ctrl Pts',(-0.0511499728070136,0.150892692640473,
0.00480048182004178));
#17435=CARTESIAN_POINT('Ctrl Pts',(0.0963263864220051,0.126747699355464,
-0.00295949408895622));
#17436=CARTESIAN_POINT('Ctrl Pts',(0.137877280219327,0.0368777401082635,
-0.00813281136162143));
#17437=CARTESIAN_POINT('Ctrl Pts',(0.135543271642224,-0.00718047980988283,
-0.0107194699979541));
#17438=CARTESIAN_POINT('Ctrl Pts',(0.109879644719093,0.0946377159884845,
0.250719469997954));
#17439=CARTESIAN_POINT('Ctrl Pts',(0.140641550146443,0.0589214351808321,
0.248132811361621));
#17440=CARTESIAN_POINT('Ctrl Pts',(0.164243388176759,-0.0441942210326729,
0.242959494088956));
#17441=CARTESIAN_POINT('Ctrl Pts',(0.055362125140226,-0.160969101710661,
0.235199518179958));
#17442=CARTESIAN_POINT('Ctrl Pts',(-0.102088475326202,-0.13602926811231,
0.227439542270961));
#17443=CARTESIAN_POINT('Ctrl Pts',(-0.169930093363525,0.00813139225995705,
0.219679566361962));
#17444=CARTESIAN_POINT('Ctrl Pts',(-0.0885810019960112,0.145257558931755,
0.211919590452965));
#17445=CARTESIAN_POINT('Ctrl Pts',(0.0705300022856002,0.154806449085219,
0.204159614543967));
#17446=CARTESIAN_POINT('Ctrl Pts',(0.167724284255384,0.0284781603319641,
0.196399638634969));
#17447=CARTESIAN_POINT('Ctrl Pts',(0.117670998255967,-0.122866343258294,
0.188639662725971));
#17448=CARTESIAN_POINT('Ctrl Pts',(-0.0356859920336591,-0.166337644224695,
0.180879686816973));
#17449=CARTESIAN_POINT('Ctrl Pts',(-0.157714277389017,-0.0637839670800676,
0.173119710907975));
#17450=CARTESIAN_POINT('Ctrl Pts',(-0.141283808251885,0.0947683240614489,
0.165359734998977));
#17451=CARTESIAN_POINT('Ctrl Pts',(-0.000819265566548849,0.17012162387625,
0.157599759089979));
#17452=CARTESIAN_POINT('Ctrl Pts',(0.140364559786514,0.0961244228297045,
0.149839783180981));
#17453=CARTESIAN_POINT('Ctrl Pts',(0.158321222407261,-0.0622614753404775,
0.142079807271983));
#17454=CARTESIAN_POINT('Ctrl Pts',(0.0372864568338413,-0.16598736897038,
0.134319831362986));
#17455=CARTESIAN_POINT('Ctrl Pts',(-0.116482378026109,-0.123991752606152,
0.126559855453987));
#17456=CARTESIAN_POINT('Ctrl Pts',(-0.167990437322196,0.0268572536432864,
0.11879987954499));
#17457=CARTESIAN_POINT('Ctrl Pts',(-0.0720183527756138,0.154128009733527,
0.111039903635992));
#17458=CARTESIAN_POINT('Ctrl Pts',(0.0871791483311938,0.146088660998552,
0.103279927726994));
#17459=CARTESIAN_POINT('Ctrl Pts',(0.169841505129784,0.00979680782987164,
0.0955199518179957));
#17460=CARTESIAN_POINT('Ctrl Pts',(0.103398469710631,-0.135095501656644,
0.0877599759089979));
#17461=CARTESIAN_POINT('Ctrl Pts',(-0.0538184879562023,-0.161386864625592,
0.08));
#17462=CARTESIAN_POINT('Ctrl Pts',(-0.163788539001263,-0.0459945892539838,
0.0722400240910021));
#17463=CARTESIAN_POINT('Ctrl Pts',(-0.129965899095288,0.10977507452059,
0.0644800481820042));
#17464=CARTESIAN_POINT('Ctrl Pts',(0.0179520450936897,0.169175430288133,
0.0567200722730062));
#17465=CARTESIAN_POINT('Ctrl Pts',(0.150115030399095,0.0800494771572726,
0.0489600963640084));
#17466=CARTESIAN_POINT('Ctrl Pts',(0.150480797316365,-0.0793413356316391,
0.0412001204550104));
#17467=CARTESIAN_POINT('Ctrl Pts',(0.0187574713458855,-0.169099111795828,
0.0334401445460125));
#17468=CARTESIAN_POINT('Ctrl Pts',(-0.129469733251211,-0.110362785133767,
0.0256801686370146));
#17469=CARTESIAN_POINT('Ctrl Pts',(-0.163964634349217,0.0451842589883535,
0.0179201927280167));
#17470=CARTESIAN_POINT('Ctrl Pts',(-0.0546483194245858,0.161212833824257,
0.0101602168190188));
#17471=CARTESIAN_POINT('Ctrl Pts',(0.10291452458962,0.135416470050577,0.00240024091002082));
#17472=CARTESIAN_POINT('Ctrl Pts',(0.147307246462226,0.0393999529324658,
-0.00277307636264439));
#17473=CARTESIAN_POINT('Ctrl Pts',(0.144813605913432,-0.00767158089707644,
-0.00535973499897704));
#17474=CARTESIAN_POINT('Ctrl Pts',(0.116913659442519,0.100696009035903,
0.256079204996931));
#17475=CARTESIAN_POINT('Ctrl Pts',(0.149644807637716,0.0626933279972582,
0.253492546360598));
#17476=CARTESIAN_POINT('Ctrl Pts',(0.174757532207842,-0.0470233419515556,
0.248319229087933));
#17477=CARTESIAN_POINT('Ctrl Pts',(0.0589061664806588,-0.171273640229548,
0.240559253178935));
#17478=CARTESIAN_POINT('Ctrl Pts',(-0.108623733429488,-0.144737267461644,
0.232799277269938));
#17479=CARTESIAN_POINT('Ctrl Pts',(-0.180808275411966,0.00865192846140473,
0.225039301360939));
#17480=CARTESIAN_POINT('Ctrl Pts',(-0.0942515706791253,0.154556313135293,
0.217279325451942));
#17481=CARTESIAN_POINT('Ctrl Pts',(0.0750450248431312,0.164716481511431,
0.209519349542944));
#17482=CARTESIAN_POINT('Ctrl Pts',(0.178461260043253,0.0303012077178856,
0.201759373633945));
#17483=CARTESIAN_POINT('Ctrl Pts',(0.125203781387627,-0.130731709675357,
0.193999397724948));
#17484=CARTESIAN_POINT('Ctrl Pts',(-0.0379704533096903,-0.17698585337688,
0.18623942181595));
#17485=CARTESIAN_POINT('Ctrl Pts',(-0.167810456277154,-0.0678671379413016,
0.178479445906952));
#17486=CARTESIAN_POINT('Ctrl Pts',(-0.150328180300649,0.100834978066992,
0.170719469997954));
#17487=CARTESIAN_POINT('Ctrl Pts',(-0.000871711368246156,0.181012066871201,
0.162959494088956));
#17488=CARTESIAN_POINT('Ctrl Pts',(0.149350085565286,0.102277888352765,
0.155199518179958));
#17489=CARTESIAN_POINT('Ctrl Pts',(0.168456255263351,-0.0662471829332422,
0.14743954227096));
#17490=CARTESIAN_POINT('Ctrl Pts',(0.0396733728729688,-0.17661315503135,
0.139679566361963));
#17491=CARTESIAN_POINT('Ctrl Pts',(-0.123939070884463,-0.131929162812062,
0.131919590452964));
#17492=CARTESIAN_POINT('Ctrl Pts',(-0.178744451066417,0.0285765376657333,
0.124159614543967));
#17493=CARTESIAN_POINT('Ctrl Pts',(-0.0766286530280003,0.163994611436961,
0.116399638634969));
#17494=CARTESIAN_POINT('Ctrl Pts',(0.0927599764682439,0.155440618724813,
0.108639662725971));
#17495=CARTESIAN_POINT('Ctrl Pts',(0.180714016146597,0.0104239566588842,
0.100879686816973));
#17496=CARTESIAN_POINT('Ctrl Pts',(0.11001758793024,-0.143743725357685,
0.093119710907975));
#17497=CARTESIAN_POINT('Ctrl Pts',(-0.0572637123892103,-0.171718146500831,
0.0853597349989769));
#17498=CARTESIAN_POINT('Ctrl Pts',(-0.174273565575645,-0.048938961879483,
0.0775997590899791));
#17499=CARTESIAN_POINT('Ctrl Pts',(-0.138285748054726,0.11680239511684,
0.0698397831809812));
#17500=CARTESIAN_POINT('Ctrl Pts',(0.0191012565771036,0.180005302104073,
0.0620798072719832));
#17501=CARTESIAN_POINT('Ctrl Pts',(0.159724738700703,0.0851738948996701,
0.0543198313629854));
#17502=CARTESIAN_POINT('Ctrl Pts',(0.160113920417758,-0.0844204212478698,
0.0465598554539874));
#17503=CARTESIAN_POINT('Ctrl Pts',(0.0199582426985643,-0.179924098035372,
0.0387998795449896));
#17504=CARTESIAN_POINT('Ctrl Pts',(-0.137757819841364,-0.117427728395404,
0.0310399036359917));
#17505=CARTESIAN_POINT('Ctrl Pts',(-0.174460933778308,0.0480767578110765,
0.0232799277269937));
#17506=CARTESIAN_POINT('Ctrl Pts',(-0.0581466660421577,0.171532975008042,
0.0155199518179959));
#17507=CARTESIAN_POINT('Ctrl Pts',(0.109502662757235,0.144085240745689,
0.00775997590899784));
#17508=CARTESIAN_POINT('Ctrl Pts',(0.156737212705124,0.0419221657566679,
0.00258665863633264));
#17509=CARTESIAN_POINT('Ctrl Pts',(0.15408394018464,-0.00816268198427004,
0.));
#17510=CARTESIAN_POINT('Ctrl Pts',(0.15408394018464,-0.00816268198427004,
0.));
#17511=CARTESIAN_POINT('Ctrl Pts',(0.153697863146473,0.00250812953454787,
1.45220469349306E-17));
#17512=CARTESIAN_POINT('Ctrl Pts',(0.152123106309386,0.0130673133993916,
-2.32988231788825E-17));
#17513=CARTESIAN_POINT('Ctrl Pts',(0.149466152202855,0.0233620190894148,
-6.07153216591882E-17));
#17514=CARTESIAN_POINT('Ctrl Pts',(0.14793019248835,0.0293132898222067,
-8.23454409684948E-17));
#17515=CARTESIAN_POINT('Ctrl Pts',(0.146031563681721,0.0351760135160456,
3.17823908273165E-17));
#17516=CARTESIAN_POINT('Ctrl Pts',(0.143784059453749,0.0409171473780902,
6.24500451351651E-17));
#17517=CARTESIAN_POINT('Ctrl Pts',(0.142595904075608,0.0439522291322952,
7.86626679846993E-17));
#17518=CARTESIAN_POINT('Ctrl Pts',(0.141309213132582,0.0469553015723855,
1.03399090950918E-16));
#17519=CARTESIAN_POINT('Ctrl Pts',(0.13992871365498,0.0499144025840292,
1.00613961606655E-16));
#17520=CARTESIAN_POINT('Ctrl Pts',(0.135493978469587,0.0594202586791481,
9.16669744478229E-17));
#17521=CARTESIAN_POINT('Ctrl Pts',(0.130119641392827,0.0684241765595774,
5.76730757846686E-17));
#17522=CARTESIAN_POINT('Ctrl Pts',(0.123887660540245,0.0767683201192124,
1.38777878078145E-16));
#17523=CARTESIAN_POINT('Ctrl Pts',(0.120656388342022,0.0810947453345699,
1.808305895663E-16));
#17524=CARTESIAN_POINT('Ctrl Pts',(0.117193874983239,0.0852432898306738,
1.062697842984E-16));
#17525=CARTESIAN_POINT('Ctrl Pts',(0.11350808038867,0.0891875047540603,
1.14491749414469E-16));
#17526=CARTESIAN_POINT('Ctrl Pts',(0.110158526423333,0.0927719043720516,
1.21963656801269E-16));
#17527=CARTESIAN_POINT('Ctrl Pts',(0.106618991420749,0.0961915975683434,
1.17223950247179E-16));
#17528=CARTESIAN_POINT('Ctrl Pts',(0.102922970874274,0.0994011657423757,
1.02348685082632E-16));
#17529=CARTESIAN_POINT('Ctrl Pts',(0.0973787571548163,0.104215676830788,
8.00350512245867E-17));
#17530=CARTESIAN_POINT('Ctrl Pts',(0.0914754811895955,0.108568278221023,
6.56075743842472E-17));
#17531=CARTESIAN_POINT('Ctrl Pts',(0.0852365492443714,0.11239450959967,
3.29597460435593E-17));
#17532=CARTESIAN_POINT('Ctrl Pts',(0.0787787796913796,0.116354950379705,
-7.26807264206779E-19));
#17533=CARTESIAN_POINT('Ctrl Pts',(0.0719608771003193,0.11975150351845,
7.81983513604452E-17));
#17534=CARTESIAN_POINT('Ctrl Pts',(0.0648645680501024,0.122569786811788,
1.05818132034585E-16));
#17535=CARTESIAN_POINT('Ctrl Pts',(0.0619760396963809,0.123716959397427,
1.17060669392563E-16));
#17536=CARTESIAN_POINT('Ctrl Pts',(0.0590419697559043,0.124767587801255,
-1.70921410850511E-17));
#17537=CARTESIAN_POINT('Ctrl Pts',(0.0560804949635964,0.12571697313192,
-8.67361737988404E-19));
#17538=CARTESIAN_POINT('Ctrl Pts',(0.0481895916857994,0.128246627558523,
4.23638569993146E-17));
#17539=CARTESIAN_POINT('Ctrl Pts',(0.040081547172159,0.13006877931966,2.48189907303608E-17));
#17540=CARTESIAN_POINT('Ctrl Pts',(0.0318655688619291,0.131172622122806,
0.));
#17541=CARTESIAN_POINT('Ctrl Pts',(0.0267717292715239,0.131856995664207,
-1.5387571972871E-17));
#17542=CARTESIAN_POINT('Ctrl Pts',(0.0216363184326117,0.132264755542675,
5.61228976213782E-17));
#17543=CARTESIAN_POINT('Ctrl Pts',(0.0164863123329273,0.132388468809724,
3.03576608295941E-17));
#17544=CARTESIAN_POINT('Ctrl Pts',(0.0120733572364389,0.13249447666326,
8.27985532573229E-18));
#17545=CARTESIAN_POINT('Ctrl Pts',(0.00764667637530932,0.132391154756805,
7.9933444120104E-17));
#17546=CARTESIAN_POINT('Ctrl Pts',(0.00324855819595315,0.132074892239241,
9.62771529167128E-17));
#17547=CARTESIAN_POINT('Ctrl Pts',(-0.00215998367955725,0.131685971569047,
1.16375665467493E-16));
#17548=CARTESIAN_POINT('Ctrl Pts',(-0.00753310453775717,0.130975837616781,
1.12286849362194E-16));
#17549=CARTESIAN_POINT('Ctrl Pts',(-0.0128378223015392,0.129936202211006,
1.27068494615301E-16));
#17550=CARTESIAN_POINT('Ctrl Pts',(-0.0180922709275414,0.128906418710228,
1.41710064449709E-16));
#17551=CARTESIAN_POINT('Ctrl Pts',(-0.023283936630727,0.12755123862641,
1.19281234835921E-16));
#17552=CARTESIAN_POINT('Ctrl Pts',(-0.028350637156304,0.125868914531291,
9.19403442267708E-17));
#17553=CARTESIAN_POINT('Ctrl Pts',(-0.0326437071621008,0.124443463179602,
6.87741127091605E-17));
#17554=CARTESIAN_POINT('Ctrl Pts',(-0.0368509055758185,0.122782751372096,
3.08039683582783E-17));
#17555=CARTESIAN_POINT('Ctrl Pts',(-0.0409513668396969,0.120880349084932,
-1.95156391047391E-18));
#17556=CARTESIAN_POINT('Ctrl Pts',(-0.0436523616789034,0.119627226953286,
-2.45035827619675E-17));
#17557=CARTESIAN_POINT('Ctrl Pts',(-0.0463070048384274,0.118269169850402,
-4.56986185075063E-18));
#17558=CARTESIAN_POINT('Ctrl Pts',(-0.0489111879062984,0.116810626195002,
-1.73472347597681E-18));
#17559=CARTESIAN_POINT('Ctrl Pts',(0.0958116152722397,0.0825211298936481,
0.24));
#17560=CARTESIAN_POINT('Ctrl Pts',(0.102494250906434,0.0762804363331629,
0.24));
#17561=CARTESIAN_POINT('Ctrl Pts',(0.108399952301676,0.0693089192431419,
0.24));
#17562=CARTESIAN_POINT('Ctrl Pts',(0.113520383394708,0.0617855200816623,
0.24));
#17563=CARTESIAN_POINT('Ctrl Pts',(0.11760088593285,0.0557900777417299,
0.24));
#17564=CARTESIAN_POINT('Ctrl Pts',(0.1211824537664,0.0494427873910869,0.24));
#17565=CARTESIAN_POINT('Ctrl Pts',(0.124247292533427,0.0428169095598754,
0.24));
#17566=CARTESIAN_POINT('Ctrl Pts',(0.125635784531567,0.0398151273949318,
0.24));
#17567=CARTESIAN_POINT('Ctrl Pts',(0.126914357096627,0.0367636074968772,
0.24));
#17568=CARTESIAN_POINT('Ctrl Pts',(0.128080244072735,0.0336751552254939,
0.24));
#17569=CARTESIAN_POINT('Ctrl Pts',(0.13155694143068,0.024465331227027,0.24));
#17570=CARTESIAN_POINT('Ctrl Pts',(0.134041462136676,0.0149150332268467,
0.24));
#17571=CARTESIAN_POINT('Ctrl Pts',(0.135496608205084,0.00520422800883078,
0.24));
#17572=CARTESIAN_POINT('Ctrl Pts',(0.136052940597398,0.00149158663520877,
0.24));
#17573=CARTESIAN_POINT('Ctrl Pts',(0.136458356591543,-0.00224482315054724,
0.24));
#17574=CARTESIAN_POINT('Ctrl Pts',(0.136708928272429,-0.00599574054845843,
0.24));
#17575=CARTESIAN_POINT('Ctrl Pts',(0.136894600108428,-0.00877514370161729,
0.24));
#17576=CARTESIAN_POINT('Ctrl Pts',(0.136994942037659,-0.0115613689854128,
0.24));
#17577=CARTESIAN_POINT('Ctrl Pts',(0.137008733057845,-0.0143405417274864,
0.24));
#17578=CARTESIAN_POINT('Ctrl Pts',(0.137045731231951,-0.0217964308202384,
0.24));
#17579=CARTESIAN_POINT('Ctrl Pts',(0.136462408227525,-0.0292204075226799,
0.24));
#17580=CARTESIAN_POINT('Ctrl Pts',(0.135240454646173,-0.0365388974416549,
0.24));
#17581=CARTESIAN_POINT('Ctrl Pts',(0.134058793448489,-0.0436160693529878,
0.24));
#17582=CARTESIAN_POINT('Ctrl Pts',(0.132280018312676,-0.050595007513092,
0.24));
#17583=CARTESIAN_POINT('Ctrl Pts',(0.129952822193542,-0.0574290655609092,
0.24));
#17584=CARTESIAN_POINT('Ctrl Pts',(0.128850070284018,-0.0606674134165377,
0.24));
#17585=CARTESIAN_POINT('Ctrl Pts',(0.127623182384127,-0.0638741644409745,
0.24));
#17586=CARTESIAN_POINT('Ctrl Pts',(0.126284110088584,-0.067028198101918,
0.24));
#17587=CARTESIAN_POINT('Ctrl Pts',(0.122654675969015,-0.0755769205431157,
0.24));
#17588=CARTESIAN_POINT('Ctrl Pts',(0.118195290975453,-0.0837663478860722,
0.24));
#17589=CARTESIAN_POINT('Ctrl Pts',(0.113014989178579,-0.0915013065162071,
0.24));
#17590=CARTESIAN_POINT('Ctrl Pts',(0.108985931714537,-0.0975172866704144,
0.24));
#17591=CARTESIAN_POINT('Ctrl Pts',(0.104519884911976,-0.103258562704539,
0.24));
#17592=CARTESIAN_POINT('Ctrl Pts',(0.0996546828651377,-0.108675969178894,
0.24));
#17593=CARTESIAN_POINT('Ctrl Pts',(0.0972822643803542,-0.11131765910988,
0.24));
#17594=CARTESIAN_POINT('Ctrl Pts',(0.09482095240722,-0.113875293456495,
0.24));
#17595=CARTESIAN_POINT('Ctrl Pts',(0.0922773332174137,-0.116342466058553,
0.24));
#17596=CARTESIAN_POINT('Ctrl Pts',(0.0868426048671788,-0.121613857680014,
0.24));
#17597=CARTESIAN_POINT('Ctrl Pts',(0.0810310485854155,-0.126474759557936,
0.24));
#17598=CARTESIAN_POINT('Ctrl Pts',(0.0748870600798396,-0.130870957562724,
0.24));
#17599=CARTESIAN_POINT('Ctrl Pts',(0.0715378781224404,-0.133267392228159,
0.24));
#17600=CARTESIAN_POINT('Ctrl Pts',(0.0680912231566627,-0.135524142754832,
0.24));
#17601=CARTESIAN_POINT('Ctrl Pts',(0.0645638484115253,-0.13762659390894,
0.24));
#17602=CARTESIAN_POINT('Ctrl Pts',(0.0598451535113139,-0.140439117742,0.24));
#17603=CARTESIAN_POINT('Ctrl Pts',(0.0549775790306604,-0.142978967531553,
0.24));
#17604=CARTESIAN_POINT('Ctrl Pts',(0.0499773507040556,-0.145225083935062,
0.24));
#17605=CARTESIAN_POINT('Ctrl Pts',(0.0466920976074369,-0.146700828718701,
0.24));
#17606=CARTESIAN_POINT('Ctrl Pts',(0.0433495270099635,-0.148049731670784,
0.24));
#17607=CARTESIAN_POINT('Ctrl Pts',(0.039956549802796,-0.149273502906639,
0.24));
#17608=CARTESIAN_POINT('Ctrl Pts',(-0.126296536029262,-6.10717992316628E-5,
0.159341967361942));
#17609=CARTESIAN_POINT('Ctrl Pts',(-0.12637083907321,-0.0163056929409037,
0.160361391877968));
#17610=CARTESIAN_POINT('Ctrl Pts',(-0.12344809088261,-0.0325245895549842,
0.161380816393994));
#17611=CARTESIAN_POINT('Ctrl Pts',(-0.117399968681154,-0.0474794518833934,
0.162400240910021));
#17612=CARTESIAN_POINT('Ctrl Pts',(-0.102053636235694,-0.0854254922118417,
0.164986899546353));
#17613=CARTESIAN_POINT('Ctrl Pts',(-0.0665853528586453,-0.115233359066084,
0.167573558182686));
#17614=CARTESIAN_POINT('Ctrl Pts',(-0.0265641275910804,-0.123819689910512,
0.170160216819019));
#17615=CARTESIAN_POINT('Ctrl Pts',(0.0134570976764845,-0.13240602075494,
0.172746875455351));
#17616=CARTESIAN_POINT('Ctrl Pts',(0.058031264834566,-0.119770815589554,
0.175333534091684));
#17617=CARTESIAN_POINT('Ctrl Pts',(0.0875924985281064,-0.0914586003428122,
0.177920192728017));
#17618=CARTESIAN_POINT('Ctrl Pts',(0.117153732221647,-0.0631463850960709,
0.180506851364349));
#17619=CARTESIAN_POINT('Ctrl Pts',(0.131702032450646,-0.0191571597679751,
0.183093510000682));
#17620=CARTESIAN_POINT('Ctrl Pts',(0.124851119980295,0.0211965060081854,
0.185680168637015));
#17621=CARTESIAN_POINT('Ctrl Pts',(0.118000207509943,0.0615501717843459,
0.188266827273347));
#17622=CARTESIAN_POINT('Ctrl Pts',(0.0897500823402403,0.0982682780085711,
0.19085348590968));
#17623=CARTESIAN_POINT('Ctrl Pts',(0.0525017161220023,0.115239608835997,
0.193440144546013));
#17624=CARTESIAN_POINT('Ctrl Pts',(0.0152533499037644,0.132210939663423,
0.196026803182345));
#17625=CARTESIAN_POINT('Ctrl Pts',(-0.030993257363009,0.129435495094051,
0.198613461818678));
#17626=CARTESIAN_POINT('Ctrl Pts',(-0.0659388717692058,0.108119484364762,
0.20120012045501));
#17627=CARTESIAN_POINT('Ctrl Pts',(-0.100884486175403,0.0868034736354726,
0.203786779091343));
#17628=CARTESIAN_POINT('Ctrl Pts',(-0.124529107721023,0.0469468967462671,
0.206373437727676));
#17629=CARTESIAN_POINT('Ctrl Pts',(-0.126492123469331,0.00606801008988057,
0.208960096364008));
#17630=CARTESIAN_POINT('Ctrl Pts',(-0.126588724127832,0.00405634646811867,
0.209087386696653));
#17631=CARTESIAN_POINT('Ctrl Pts',(-0.126632819376787,0.00204220716288977,
0.209214677029297));
#17632=CARTESIAN_POINT('Ctrl Pts',(-0.126625441102054,2.7778768752873E-5,
0.209341967361942));
#17633=CARTESIAN_POINT('Ctrl Pts',(-0.0398513841857245,-0.149064942821851,
0.24));
#17634=CARTESIAN_POINT('Ctrl Pts',(-0.0883048112969314,-0.136111285829332,
0.237413341363667));
#17635=CARTESIAN_POINT('Ctrl Pts',(-0.170871437255804,-0.0596187094618861,
0.232240024091002));
#17636=CARTESIAN_POINT('Ctrl Pts',(-0.145169204726118,0.108307533342445,
0.224480048182004));
#17637=CARTESIAN_POINT('Ctrl Pts',(0.00818767200092134,0.180778621679153,
0.216720072273006));
#17638=CARTESIAN_POINT('Ctrl Pts',(0.154249898498561,0.0947283641859207,
0.208960096364008));
#17639=CARTESIAN_POINT('Ctrl Pts',(0.164950538597243,-0.0745810526211722,
0.201200120455011));
#17640=CARTESIAN_POINT('Ctrl Pts',(0.0308106631569891,-0.178364693496558,
0.193440144546012));
#17641=CARTESIAN_POINT('Ctrl Pts',(-0.13036283225522,-0.125587074703769,
0.185680168637015));
#17642=CARTESIAN_POINT('Ctrl Pts',(-0.17709781441264,0.03745832727601,0.177920192728017));
#17643=CARTESIAN_POINT('Ctrl Pts',(-0.0683530255288039,0.167611467503216,
0.170160216819019));
#17644=CARTESIAN_POINT('Ctrl Pts',(0.100397202365132,0.150621028353064,
0.162400240910021));
#17645=CARTESIAN_POINT('Ctrl Pts',(0.18100910679194,0.00139719974911195,
0.154640265001023));
#17646=CARTESIAN_POINT('Ctrl Pts',(0.102711092909207,-0.149052183789333,
0.146880289092025));
#17647=CARTESIAN_POINT('Ctrl Pts',(-0.0657574679958034,-0.168648048308422,
0.139120313183027));
#17648=CARTESIAN_POINT('Ctrl Pts',(-0.176497206835689,-0.0401861834345609,
0.131360337274029));
#17649=CARTESIAN_POINT('Ctrl Pts',(-0.132288575936487,0.123555290563421,
0.123600361365031));
#17650=CARTESIAN_POINT('Ctrl Pts',(0.0280571680938306,0.178826694862324,
0.115840385456033));
#17651=CARTESIAN_POINT('Ctrl Pts',(0.163771354656592,0.0771047007047774,
0.108080409547035));
#17652=CARTESIAN_POINT('Ctrl Pts',(0.155709331479018,-0.0923080778690166,
0.100320433638038));
#17653=CARTESIAN_POINT('Ctrl Pts',(0.0109489686262093,-0.180682908560435,
0.0925604577290397));
#17654=CARTESIAN_POINT('Ctrl Pts',(-0.143423754439364,-0.110434756566834,
0.0848004818200417));
#17655=CARTESIAN_POINT('Ctrl Pts',(-0.17188331593326,0.0567648465404429,
0.0770405059110439));
#17656=CARTESIAN_POINT('Ctrl Pts',(-0.0494457976037486,0.174130301808973,
0.0692805300020459));
#17657=CARTESIAN_POINT('Ctrl Pts',(0.11640175885633,0.13862511662766,0.061520554093048));
#17658=CARTESIAN_POINT('Ctrl Pts',(0.18005704388064,-0.0185795878987759,
0.0537605781840501));
#17659=CARTESIAN_POINT('Ctrl Pts',(0.0856431484406112,-0.159474177462153,
0.0460006022750521));
#17660=CARTESIAN_POINT('Ctrl Pts',(-0.0839657292871194,-0.160363143120653,
0.0382406263660544));
#17661=CARTESIAN_POINT('Ctrl Pts',(-0.179844832231877,-0.0204718628801216,
0.0304806504570563));
#17662=CARTESIAN_POINT('Ctrl Pts',(-0.117866479118068,0.137399078213474,
0.0227206745480585));
#17663=CARTESIAN_POINT('Ctrl Pts',(0.0476444145610997,0.174632482457551,
0.0149606986390605));
#17664=CARTESIAN_POINT('Ctrl Pts',(0.171219786572432,0.0585809927800803,
0.00720072273006264));
#17665=CARTESIAN_POINT('Ctrl Pts',(0.144688050375066,-0.108949473877577,
-0.000559253178935319));
#17666=CARTESIAN_POINT('Ctrl Pts',(-0.0092814439579932,-0.180735423716049,
-0.00831922908793317));
#17667=CARTESIAN_POINT('Ctrl Pts',(-0.105867686800049,-0.122947365648507,
-0.0134925463605985));
#17668=CARTESIAN_POINT('Ctrl Pts',(-0.131895903200816,-0.0800747195988904,
-0.0160792049969312));
#17669=CARTESIAN_POINT('Ctrl Pts',(-0.0374537582415196,-0.140096572423086,
0.245359734998977));
#17670=CARTESIAN_POINT('Ctrl Pts',(-0.0829920245295529,-0.127922261611689,
0.242773076362644));
#17671=CARTESIAN_POINT('Ctrl Pts',(-0.160591096949962,-0.0560317985556137,
0.237599759089979));
#17672=CARTESIAN_POINT('Ctrl Pts',(-0.13643521822445,0.101791299158848,
0.229839783180981));
#17673=CARTESIAN_POINT('Ctrl Pts',(0.00769506740980954,0.1699022237233,
0.222079807271983));
#17674=CARTESIAN_POINT('Ctrl Pts',(0.144969579481095,0.0890291096113304,
0.214319831362985));
#17675=CARTESIAN_POINT('Ctrl Pts',(0.155026424317845,-0.0700939445729984,
0.206559855453987));
#17676=CARTESIAN_POINT('Ctrl Pts',(0.0289569648011409,-0.167633527556011,
0.19879987954499));
#17677=CARTESIAN_POINT('Ctrl Pts',(-0.122519659046519,-0.118031231043151,
0.191039903635991));
#17678=CARTESIAN_POINT('Ctrl Pts',(-0.166442869216287,0.0352046776440443,
0.183279927726994));
#17679=CARTESIAN_POINT('Ctrl Pts',(-0.064240621638164,0.157527260611955,
0.175519951817996));
#17680=CARTESIAN_POINT('Ctrl Pts',(0.0943568867767351,0.141559037340679,
0.167759975908998));
#17681=CARTESIAN_POINT('Ctrl Pts',(0.170118841887737,0.00131313836865665,
0.16));
#17682=CARTESIAN_POINT('Ctrl Pts',(0.0965315639882279,-0.140084581027326,
0.152240024091002));
#17683=CARTESIAN_POINT('Ctrl Pts',(-0.0618012237018238,-0.158501476380598,
0.144480048182004));
#17684=CARTESIAN_POINT('Ctrl Pts',(-0.165878396703103,-0.0377684145673052,
0.136720072273006));
#17685=CARTESIAN_POINT('Ctrl Pts',(-0.124329541933827,0.116121687534276,
0.128960096364008));
#17686=CARTESIAN_POINT('Ctrl Pts',(0.0263691315170036,0.168067732987372,
0.12120012045501));
#17687=CARTESIAN_POINT('Ctrl Pts',(0.153918185014798,0.0724657594331675,
0.113440144546012));
#17688=CARTESIAN_POINT('Ctrl Pts',(0.146341206869619,-0.0867544378416841,
0.105680168637015));
#17689=CARTESIAN_POINT('Ctrl Pts',(0.0102902328814698,-0.169812269106107,
0.0979201927280167));
#17690=CARTESIAN_POINT('Ctrl Pts',(-0.134794781526993,-0.103790539737311,
0.0901602168190187));
#17691=CARTESIAN_POINT('Ctrl Pts',(-0.161542096774173,0.0533496359633175,
0.0824002409100209));
#17692=CARTESIAN_POINT('Ctrl Pts',(-0.0464709316213242,0.163653894581969,
0.074640265001023));
#17693=CARTESIAN_POINT('Ctrl Pts',(0.109398542213106,0.130284849835523,
0.066880289092025));
#17694=CARTESIAN_POINT('Ctrl Pts',(0.16922405906302,-0.0174617621848401,
0.0591203131830272));
#17695=CARTESIAN_POINT('Ctrl Pts',(0.0804904984426183,-0.149879543972585,
0.0513603372740291));
#17696=CARTESIAN_POINT('Ctrl Pts',(-0.0789139998409189,-0.150715025739123,
0.0436003613650314));
#17697=CARTESIAN_POINT('Ctrl Pts',(-0.169024614954586,-0.0192401899891918,
0.0358403854560333));
#17698=CARTESIAN_POINT('Ctrl Pts',(-0.110775138777956,0.12913257502003,
0.0280804095470356));
#17699=CARTESIAN_POINT('Ctrl Pts',(0.0447779273164969,0.164125861942445,
0.0203204336380375));
#17700=CARTESIAN_POINT('Ctrl Pts',(0.16091848811479,0.0550565152494576,
0.0125604577290397));
#17701=CARTESIAN_POINT('Ctrl Pts',(0.135983012131502,-0.10239461786658,
0.00480048182004171));
#17702=CARTESIAN_POINT('Ctrl Pts',(-0.00872303347143,-0.169861624730324,
-0.00295949408895612));
#17703=CARTESIAN_POINT('Ctrl Pts',(-0.0994982439886826,-0.115550337924785,
-0.00813281136162148));
#17704=CARTESIAN_POINT('Ctrl Pts',(-0.123960494032221,-0.0752570895690155,
-0.0107194699979541));
#17705=CARTESIAN_POINT('Ctrl Pts',(-0.0350561322973148,-0.13112820202432,
0.250719469997954));
#17706=CARTESIAN_POINT('Ctrl Pts',(-0.0776792377621743,-0.119733237394047,
0.248132811361621));
#17707=CARTESIAN_POINT('Ctrl Pts',(-0.150310756644121,-0.0524448876493412,
0.242959494088956));
#17708=CARTESIAN_POINT('Ctrl Pts',(-0.127701231722781,0.0952750649752511,
0.235199518179958));
#17709=CARTESIAN_POINT('Ctrl Pts',(0.00720246281869772,0.159025825767447,
0.22743954227096));
#17710=CARTESIAN_POINT('Ctrl Pts',(0.135689260463629,0.08332985503674,0.219679566361962));
#17711=CARTESIAN_POINT('Ctrl Pts',(0.145102310038447,-0.0656068365248246,
0.211919590452964));
#17712=CARTESIAN_POINT('Ctrl Pts',(0.0271032664452926,-0.156902361615465,
0.204159614543967));
#17713=CARTESIAN_POINT('Ctrl Pts',(-0.114676485837817,-0.110475387382534,
0.196399638634969));
#17714=CARTESIAN_POINT('Ctrl Pts',(-0.155787924019933,0.0329510280120788,
0.188639662725971));
#17715=CARTESIAN_POINT('Ctrl Pts',(-0.0601282177475243,0.147443053720694,
0.180879686816973));
#17716=CARTESIAN_POINT('Ctrl Pts',(0.0883165711883383,0.132497046328295,
0.173119710907975));
#17717=CARTESIAN_POINT('Ctrl Pts',(0.159228576983534,0.00122907698820117,
0.165359734998977));
#17718=CARTESIAN_POINT('Ctrl Pts',(0.0903520350672485,-0.131116978265319,
0.157599759089979));
#17719=CARTESIAN_POINT('Ctrl Pts',(-0.0578449794078444,-0.148354904452775,
0.149839783180981));
#17720=CARTESIAN_POINT('Ctrl Pts',(-0.155259586570517,-0.0353506457000499,
0.142079807271983));
#17721=CARTESIAN_POINT('Ctrl Pts',(-0.116370507931168,0.108688084505131,
0.134319831362985));
#17722=CARTESIAN_POINT('Ctrl Pts',(0.0246810949401768,0.157308771112418,
0.126559855453988));
#17723=CARTESIAN_POINT('Ctrl Pts',(0.144065015373005,0.0678268181615582,
0.118799879544989));
#17724=CARTESIAN_POINT('Ctrl Pts',(0.13697308226022,-0.0812007978143519,
0.111039903635992));
#17725=CARTESIAN_POINT('Ctrl Pts',(0.00963149713673027,-0.15894162965178,
0.103279927726994));
#17726=CARTESIAN_POINT('Ctrl Pts',(-0.126165808614623,-0.0971463229077874,
0.0955199518179957));
#17727=CARTESIAN_POINT('Ctrl Pts',(-0.151200877615086,0.0499344253861922,
0.087759975908998));
#17728=CARTESIAN_POINT('Ctrl Pts',(-0.0434960656388994,0.153177487354966,
0.08));
#17729=CARTESIAN_POINT('Ctrl Pts',(0.102395325569881,0.121944583043386,
0.072240024091002));
#17730=CARTESIAN_POINT('Ctrl Pts',(0.158391074245402,-0.0163439364709043,
0.0644800481820042));
#17731=CARTESIAN_POINT('Ctrl Pts',(0.0753378484446251,-0.140284910483017,
0.0567200722730062));
#17732=CARTESIAN_POINT('Ctrl Pts',(-0.0738622703947183,-0.141066908357593,
0.0489600963640083));
#17733=CARTESIAN_POINT('Ctrl Pts',(-0.158204397677296,-0.018008517098262,
0.0412001204550104));
#17734=CARTESIAN_POINT('Ctrl Pts',(-0.103683798437843,0.120866071826586,
0.0334401445460125));
#17735=CARTESIAN_POINT('Ctrl Pts',(0.0419114400718942,0.153619241427338,
0.0256801686370146));
#17736=CARTESIAN_POINT('Ctrl Pts',(0.150617189657149,0.051532037718835,
0.0179201927280167));
#17737=CARTESIAN_POINT('Ctrl Pts',(0.127277973887939,-0.0958397618555833,
0.0101602168190187));
#17738=CARTESIAN_POINT('Ctrl Pts',(-0.00816462298486686,-0.1589878257446,
0.00240024091002091));
#17739=CARTESIAN_POINT('Ctrl Pts',(-0.0931288011773165,-0.108153310201063,
-0.00277307636264444));
#17740=CARTESIAN_POINT('Ctrl Pts',(-0.116025084863626,-0.0704394595391406,
-0.00535973499897709));
#17741=CARTESIAN_POINT('Ctrl Pts',(-0.0326585063531099,-0.122159831625555,
0.256079204996931));
#17742=CARTESIAN_POINT('Ctrl Pts',(-0.0723664509947957,-0.111544213176404,
0.253492546360598));
#17743=CARTESIAN_POINT('Ctrl Pts',(-0.140030416338279,-0.0488579767430688,
0.248319229087933));
#17744=CARTESIAN_POINT('Ctrl Pts',(-0.118967245221113,0.0887588307916541,
0.240559253178936));
#17745=CARTESIAN_POINT('Ctrl Pts',(0.00670985822758596,0.148149427811594,
0.232799277269937));
#17746=CARTESIAN_POINT('Ctrl Pts',(0.126408941446163,0.0776306004621497,
0.225039301360939));
#17747=CARTESIAN_POINT('Ctrl Pts',(0.13517819575905,-0.0611197284766509,
0.217279325451942));
#17748=CARTESIAN_POINT('Ctrl Pts',(0.0252495680894444,-0.146171195674918,
0.209519349542944));
#17749=CARTESIAN_POINT('Ctrl Pts',(-0.106833312629116,-0.102919543721916,
0.201759373633946));
#17750=CARTESIAN_POINT('Ctrl Pts',(-0.14513297882358,0.0306973783801131,
0.193999397724948));
#17751=CARTESIAN_POINT('Ctrl Pts',(-0.0560158138568844,0.137358846829434,
0.18623942181595));
#17752=CARTESIAN_POINT('Ctrl Pts',(0.0822762555999414,0.12343505531591,
0.178479445906952));
#17753=CARTESIAN_POINT('Ctrl Pts',(0.148338312079331,0.00114501560774606,
0.170719469997954));
#17754=CARTESIAN_POINT('Ctrl Pts',(0.0841725061462688,-0.122149375503312,
0.162959494088956));
#17755=CARTESIAN_POINT('Ctrl Pts',(-0.0538887351138648,-0.138208332524951,
0.155199518179959));
#17756=CARTESIAN_POINT('Ctrl Pts',(-0.144640776437932,-0.0329328768327946,
0.14743954227096));
#17757=CARTESIAN_POINT('Ctrl Pts',(-0.108411473928508,0.101254481475986,
0.139679566361963));
#17758=CARTESIAN_POINT('Ctrl Pts',(0.0229930583633497,0.146549809237466,
0.131919590452964));
#17759=CARTESIAN_POINT('Ctrl Pts',(0.134211845731212,0.0631878768899486,
0.124159614543967));
#17760=CARTESIAN_POINT('Ctrl Pts',(0.127604957650822,-0.0756471577870196,
0.116399638634969));
#17761=CARTESIAN_POINT('Ctrl Pts',(0.00897276139199077,-0.148070990197453,
0.108639662725971));
#17762=CARTESIAN_POINT('Ctrl Pts',(-0.117536835702253,-0.0905021060782641,
0.100879686816973));
#17763=CARTESIAN_POINT('Ctrl Pts',(-0.140859658455999,0.0465192148090667,
0.0931197109079749));
#17764=CARTESIAN_POINT('Ctrl Pts',(-0.0405211996564747,0.142701080127962,
0.0853597349989771));
#17765=CARTESIAN_POINT('Ctrl Pts',(0.0953921089266558,0.113604316251249,
0.077599759089979));
#17766=CARTESIAN_POINT('Ctrl Pts',(0.147558089427783,-0.0152261107569683,
0.0698397831809813));
#17767=CARTESIAN_POINT('Ctrl Pts',(0.070185198446632,-0.130690276993449,
0.0620798072719832));
#17768=CARTESIAN_POINT('Ctrl Pts',(-0.0688105409485176,-0.131418790976063,
0.0543198313629854));
#17769=CARTESIAN_POINT('Ctrl Pts',(-0.147384180400005,-0.0167768442073323,
0.0465598554539874));
#17770=CARTESIAN_POINT('Ctrl Pts',(-0.0965924580977301,0.112599568633142,
0.0387998795449896));
#17771=CARTESIAN_POINT('Ctrl Pts',(0.0390449528272914,0.143112620912232,
0.0310399036359916));
#17772=CARTESIAN_POINT('Ctrl Pts',(0.140315891199508,0.0480075601882123,
0.0232799277269937));
#17773=CARTESIAN_POINT('Ctrl Pts',(0.118572935644375,-0.0892849058445864,
0.0155199518179958));
#17774=CARTESIAN_POINT('Ctrl Pts',(-0.00760621249830358,-0.148114026758875,
0.00775997590899793));
#17775=CARTESIAN_POINT('Ctrl Pts',(-0.0867593583659504,-0.100756282477341,
0.00258665863633259));
#17776=CARTESIAN_POINT('Ctrl Pts',(-0.108089675695031,-0.0656218295092657,
-5.55111512312578E-17));
#17777=CARTESIAN_POINT('Ctrl Pts',(-0.108089675695031,-0.0656218295092657,
-5.55111512312578E-17));
#17778=CARTESIAN_POINT('Ctrl Pts',(-0.104219465379748,-0.0739058869203245,
-4.02841154597017E-17));
#17779=CARTESIAN_POINT('Ctrl Pts',(-0.0994141168358061,-0.0816768736924768,
-5.16144647363644E-17));
#17780=CARTESIAN_POINT('Ctrl Pts',(-0.0938412360364922,-0.088871564406415,
-3.81639164714898E-17));
#17781=CARTESIAN_POINT('Ctrl Pts',(-0.0894001862863345,-0.094605040600905,
-2.74451237748006E-17));
#17782=CARTESIAN_POINT('Ctrl Pts',(-0.0844703330957707,-0.0999727304469881,
3.12377098840079E-17));
#17783=CARTESIAN_POINT('Ctrl Pts',(-0.0791158513129458,-0.104935071387697,
-1.21430643318376E-17));
#17784=CARTESIAN_POINT('Ctrl Pts',(-0.0766900604813501,-0.107183206995485,
-3.17962611543325E-17));
#17785=CARTESIAN_POINT('Ctrl Pts',(-0.0741829996358932,-0.109342173006691,
4.83248416902999E-17));
#17786=CARTESIAN_POINT('Ctrl Pts',(-0.0716059924168524,-0.111405381598006,
5.3776427755281E-17));
#17787=CARTESIAN_POINT('Ctrl Pts',(-0.0639212992135713,-0.117557915794061,
7.00331794132204E-17));
#17788=CARTESIAN_POINT('Ctrl Pts',(-0.0556061968393146,-0.12287204611112,
-5.69073736333764E-18));
#17789=CARTESIAN_POINT('Ctrl Pts',(-0.0468203466856493,-0.127256781127915,
5.55111512312578E-17));
#17790=CARTESIAN_POINT('Ctrl Pts',(-0.0434613267337519,-0.12893315986732,
7.89099528597243E-17));
#17791=CARTESIAN_POINT('Ctrl Pts',(-0.0400330653128497,-0.130473352587733,
3.97002991909352E-17));
#17792=CARTESIAN_POINT('Ctrl Pts',(-0.0365431560942257,-0.131870761756357,
6.59194920871187E-17));
#17793=CARTESIAN_POINT('Ctrl Pts',(-0.0339571636773035,-0.13290622981212,
8.5347686277821E-17));
#17794=CARTESIAN_POINT('Ctrl Pts',(-0.0313383144727484,-0.133862652235137,
-2.74403076010104E-17));
#17795=CARTESIAN_POINT('Ctrl Pts',(-0.0286994266230122,-0.134734580282325,
-2.42861286636753E-17));
#17796=CARTESIAN_POINT('Ctrl Pts',(-0.0216199050576346,-0.137073760181214,
-1.58242011095522E-17));
#17797=CARTESIAN_POINT('Ctrl Pts',(-0.0143790427459088,-0.138813119073991,
5.80198461902811E-17));
#17798=CARTESIAN_POINT('Ctrl Pts',(-0.0070411538297537,-0.139912507657099,
6.93889390390723E-17));
#17799=CARTESIAN_POINT('Ctrl Pts',(5.47883476400097E-5,-0.140975646920361,
8.02325614020808E-17));
#17800=CARTESIAN_POINT('Ctrl Pts',(0.00724182591717642,-0.141440539972256,
1.32011341321413E-16));
#17801=CARTESIAN_POINT('Ctrl Pts',(0.0144605478337719,-0.141339082434075,
1.61329283265843E-16));
#17802=CARTESIAN_POINT('Ctrl Pts',(0.0178811722145177,-0.141291006315792,
1.75221724083914E-16));
#17803=CARTESIAN_POINT('Ctrl Pts',(0.021310106848269,-0.141115105569205,
1.85534911235541E-16));
#17804=CARTESIAN_POINT('Ctrl Pts',(0.0247235715439624,-0.140816220288761,
1.71737624121704E-16));
#17805=CARTESIAN_POINT('Ctrl Pts',(0.0339754553361668,-0.140006119078294,
1.34341339582434E-16));
#17806=CARTESIAN_POINT('Ctrl Pts',(0.0431421008898472,-0.138295657968001,
8.04496487960062E-17));
#17807=CARTESIAN_POINT('Ctrl Pts',(0.0520992976556894,-0.135759125106636,
3.20923843055709E-17));
#17808=CARTESIAN_POINT('Ctrl Pts',(0.0590658916121619,-0.13378629867842,
-5.518202506064E-18));
#17809=CARTESIAN_POINT('Ctrl Pts',(0.0659062642374416,-0.131312982137409,
7.87850579480063E-17));
#17810=CARTESIAN_POINT('Ctrl Pts',(0.0725619642951071,-0.128359965266718,
7.63278329429795E-17));
#17811=CARTESIAN_POINT('Ctrl Pts',(0.0758074813473741,-0.126919986522721,
7.51296170399226E-17));
#17812=CARTESIAN_POINT('Ctrl Pts',(0.0790005264283722,-0.125369490597537,
8.38688896655138E-17));
#17813=CARTESIAN_POINT('Ctrl Pts',(0.0821329715644795,-0.123712761836801,
7.24247051220317E-17));
#17814=CARTESIAN_POINT('Ctrl Pts',(0.0888257654942848,-0.120172989003949,
4.79730178566093E-17));
#17815=CARTESIAN_POINT('Ctrl Pts',(0.0952446087626691,-0.116147988031934,
8.96774285244103E-17));
#17816=CARTESIAN_POINT('Ctrl Pts',(0.101324221742587,-0.111663228753314,
8.28330459778925E-17));
#17817=CARTESIAN_POINT('Ctrl Pts',(0.104638321741973,-0.109218510516871,
7.91020571356516E-17));
#17818=CARTESIAN_POINT('Ctrl Pts',(0.107849695272814,-0.106637925639498,
3.17151869302413E-17));
#17819=CARTESIAN_POINT('Ctrl Pts',(0.110939265073957,-0.10393289123317,
1.53956708492942E-17));
#17820=CARTESIAN_POINT('Ctrl Pts',(0.115072333360666,-0.100314234708527,
-6.43574216607592E-18));
#17821=CARTESIAN_POINT('Ctrl Pts',(0.118992075260627,-0.0964697210975667,
5.54296751400654E-17));
#17822=CARTESIAN_POINT('Ctrl Pts',(0.122673447199167,-0.0924082746861152,
3.52365706057789E-17));
#17823=CARTESIAN_POINT('Ctrl Pts',(0.125092164655522,-0.0897398425098966,
2.31620156359627E-17));
#17824=CARTESIAN_POINT('Ctrl Pts',(0.127407959881093,-0.0869777021544565,
-4.01489640485901E-17));
#17825=CARTESIAN_POINT('Ctrl Pts',(0.129620323775263,-0.0841289546921697,
-3.98986399474666E-17));
#17826=CARTESIAN_POINT('Ctrl Pts',(-0.126471935391749,0.000101176582396995,
0.195658032638058));
#17827=CARTESIAN_POINT('Ctrl Pts',(-0.126547267107008,0.00888033934128026,
0.195105154333688));
#17828=CARTESIAN_POINT('Ctrl Pts',(-0.125707148272093,0.0176451944231377,
0.194552276029318));
#17829=CARTESIAN_POINT('Ctrl Pts',(-0.12389684029672,0.0262048027713284,
0.193999397724948));
#17830=CARTESIAN_POINT('Ctrl Pts',(-0.115427257168015,0.0662512011965534,
0.191412739088615));
#17831=CARTESIAN_POINT('Ctrl Pts',(-0.0857215355124495,0.101805024012994,
0.188826080452282));
#17832=CARTESIAN_POINT('Ctrl Pts',(-0.0478199964418627,0.117261303502293,
0.18623942181595));
#17833=CARTESIAN_POINT('Ctrl Pts',(-0.0099184573712758,0.132717582991593,
0.183652763179617));
#17834=CARTESIAN_POINT('Ctrl Pts',(0.0361788991143328,0.128076319153751,
0.181066104543285));
#17835=CARTESIAN_POINT('Ctrl Pts',(0.070237920103702,0.105374013950137,
0.178479445906952));
#17836=CARTESIAN_POINT('Ctrl Pts',(0.104296941093071,0.0826717087465222,
0.175892787270619));
#17837=CARTESIAN_POINT('Ctrl Pts',(0.126317626586201,0.0419083621771342,
0.173306128634287));
#17838=CARTESIAN_POINT('Ctrl Pts',(0.126633668343922,0.000977623707263797,
0.170719469997954));
#17839=CARTESIAN_POINT('Ctrl Pts',(0.126949710101644,-0.0399531147626067,
0.168132811361621));
#17840=CARTESIAN_POINT('Ctrl Pts',(0.105561108123956,-0.08105124513296,
0.165546152725289));
#17841=CARTESIAN_POINT('Ctrl Pts',(0.0718566002584231,-0.104276803155076,
0.162959494088956));
#17842=CARTESIAN_POINT('Ctrl Pts',(0.0381520923928904,-0.127502361177192,
0.160372835452623));
#17843=CARTESIAN_POINT('Ctrl Pts',(-0.00786832136048696,-0.132855346851071,
0.157786176816291));
#17844=CARTESIAN_POINT('Ctrl Pts',(-0.0460038684578537,-0.117985930405985,
0.155199518179958));
#17845=CARTESIAN_POINT('Ctrl Pts',(-0.0841394155552204,-0.103116513960899,
0.152612859543626));
#17846=CARTESIAN_POINT('Ctrl Pts',(-0.114390095996576,-0.0680246953968468,
0.150026200907293));
#17847=CARTESIAN_POINT('Ctrl Pts',(-0.12347721913235,-0.0281142263966907,
0.14743954227096));
#17848=CARTESIAN_POINT('Ctrl Pts',(-0.125563410841138,-0.018951712774069,
0.14684570572666));
#17849=CARTESIAN_POINT('Ctrl Pts',(-0.126534167537385,-0.00953522996602069,
0.146251869182359));
#17850=CARTESIAN_POINT('Ctrl Pts',(-0.126453631260982,-0.000102348163238207,
0.145658032638058));
#17851=CARTESIAN_POINT('Ctrl Pts',(-0.0398513841857245,-0.149064942821851,
0.24));
#17852=CARTESIAN_POINT('Ctrl Pts',(-0.0498806325786677,-0.145400296738327,
0.24));
#17853=CARTESIAN_POINT('Ctrl Pts',(-0.0594363948008725,-0.140639648297949,
0.24));
#17854=CARTESIAN_POINT('Ctrl Pts',(-0.0684062055177017,-0.134931499399492,
0.24));
#17855=CARTESIAN_POINT('Ctrl Pts',(-0.0735915624001909,-0.131631676235849,
0.24));
#17856=CARTESIAN_POINT('Ctrl Pts',(-0.0785806353345173,-0.128014298080738,
0.24));
#17857=CARTESIAN_POINT('Ctrl Pts',(-0.0833462611484583,-0.124102693747304,
0.24));
#17858=CARTESIAN_POINT('Ctrl Pts',(-0.0858656342542594,-0.122034803580736,
0.24));
#17859=CARTESIAN_POINT('Ctrl Pts',(-0.0883241156266364,-0.11988309220465,
0.24));
#17860=CARTESIAN_POINT('Ctrl Pts',(-0.0907117892851122,-0.117655751751618,
0.24));
#17861=CARTESIAN_POINT('Ctrl Pts',(-0.0983819858496404,-0.110500611839494,
0.24));
#17862=CARTESIAN_POINT('Ctrl Pts',(-0.105284458416918,-0.102606966330569,
0.24));
#17863=CARTESIAN_POINT('Ctrl Pts',(-0.111294422020379,-0.0941015332659665,
0.24));
#17864=CARTESIAN_POINT('Ctrl Pts',(-0.114410577497229,-0.0896914812962706,
0.24));
#17865=CARTESIAN_POINT('Ctrl Pts',(-0.117286101138547,-0.0851164738413172,
0.24));
#17866=CARTESIAN_POINT('Ctrl Pts',(-0.119898298320422,-0.0803922539627851,
0.24));
#17867=CARTESIAN_POINT('Ctrl Pts',(-0.1222721977331,-0.0760990011896685,
0.24));
#17868=CARTESIAN_POINT('Ctrl Pts',(-0.124430744329062,-0.0716759619599862,
0.24));
#17869=CARTESIAN_POINT('Ctrl Pts',(-0.126341093034125,-0.0671690272221462,
0.24));
#17870=CARTESIAN_POINT('Ctrl Pts',(-0.129206708925078,-0.060408406100978,
0.24));
#17871=CARTESIAN_POINT('Ctrl Pts',(-0.131522065955468,-0.0534490321795157,
0.24));
#17872=CARTESIAN_POINT('Ctrl Pts',(-0.133233091500091,-0.0463330844490581,
0.24));
#17873=CARTESIAN_POINT('Ctrl Pts',(-0.135004134506116,-0.0389675313754268,
0.24));
#17874=CARTESIAN_POINT('Ctrl Pts',(-0.136127599829873,-0.0314337185245799,
0.24));
#17875=CARTESIAN_POINT('Ctrl Pts',(-0.136615064298196,-0.0238138180582873,
0.24));
#17876=CARTESIAN_POINT('Ctrl Pts',(-0.136813484749433,-0.0207121682209076,
0.24));
#17877=CARTESIAN_POINT('Ctrl Pts',(-0.136906013213758,-0.0175970392000076,
0.24));
#17878=CARTESIAN_POINT('Ctrl Pts',(-0.136893785357156,-0.0144871321155608,
0.24));
#17879=CARTESIAN_POINT('Ctrl Pts',(-0.136861203984761,-0.00620072149302863,
0.24));
#17880=CARTESIAN_POINT('Ctrl Pts',(-0.136088646936857,0.00207357465703332,
0.24));
#17881=CARTESIAN_POINT('Ctrl Pts',(-0.134599584032292,0.0102285531249486,
0.24));
#17882=CARTESIAN_POINT('Ctrl Pts',(-0.133676409755049,0.0152843948425598,
0.24));
#17883=CARTESIAN_POINT('Ctrl Pts',(-0.132477333465274,0.0202942984003417,
0.24));
#17884=CARTESIAN_POINT('Ctrl Pts',(-0.131003622030167,0.0252303138624672,
0.24));
#17885=CARTESIAN_POINT('Ctrl Pts',(-0.129740734874544,0.029460199292259,
0.24));
#17886=CARTESIAN_POINT('Ctrl Pts',(-0.128274507607502,0.0336384499732856,
0.24));
#17887=CARTESIAN_POINT('Ctrl Pts',(-0.126614574688298,0.0377237273426867,
0.24));
#17888=CARTESIAN_POINT('Ctrl Pts',(-0.124573382985647,0.042747324485064,
0.24));
#17889=CARTESIAN_POINT('Ctrl Pts',(-0.122237651925267,0.0476379767326878,
0.24));
#17890=CARTESIAN_POINT('Ctrl Pts',(-0.119609691052418,0.0523617558795304,
0.24));
#17891=CARTESIAN_POINT('Ctrl Pts',(-0.117006563775536,0.0570408964535612,
0.24));
#17892=CARTESIAN_POINT('Ctrl Pts',(-0.114113358229268,0.0615597689541448,
0.24));
#17893=CARTESIAN_POINT('Ctrl Pts',(-0.110947628485839,0.0658586917144141,
0.24));
#17894=CARTESIAN_POINT('Ctrl Pts',(-0.108265305855902,0.0695011687224882,
0.24));
#17895=CARTESIAN_POINT('Ctrl Pts',(-0.105385772272888,0.0729892759232728,
0.24));
#17896=CARTESIAN_POINT('Ctrl Pts',(-0.102309360287629,0.0763011815833395,
0.24));
#17897=CARTESIAN_POINT('Ctrl Pts',(-0.100282916666232,0.0784827457339379,
0.24));
#17898=CARTESIAN_POINT('Ctrl Pts',(-0.0981709975111385,0.0805877996091198,
0.24));
#17899=CARTESIAN_POINT('Ctrl Pts',(-0.0959791030802606,0.0826138105732947,
0.24));
#17900=CARTESIAN_POINT('Origin',(0.,0.,0.24));
#17901=CARTESIAN_POINT('',(0.158771324027147,-0.275,0.24));
#17902=CARTESIAN_POINT('',(0.317542648054294,0.,0.24));
#17903=CARTESIAN_POINT('',(0.158771324027147,-0.275,0.24));
#17904=CARTESIAN_POINT('',(0.158771324027147,0.275,0.24));
#17905=CARTESIAN_POINT('',(0.317542648054294,0.,0.24));
#17906=CARTESIAN_POINT('',(-0.158771324027147,0.275,0.24));
#17907=CARTESIAN_POINT('',(0.158771324027147,0.275,0.24));
#17908=CARTESIAN_POINT('',(-0.317542648054294,5.55111512312578E-17,0.24));
#17909=CARTESIAN_POINT('',(-0.158771324027147,0.275,0.24));
#17910=CARTESIAN_POINT('',(-0.158771324027147,-0.275,0.24));
#17911=CARTESIAN_POINT('',(-0.317542648054294,3.88877587532466E-17,0.24));
#17912=CARTESIAN_POINT('',(-0.158771324027147,-0.275,0.24));
#17913=CARTESIAN_POINT('Origin',(0.,0.,0.12));
#17914=CARTESIAN_POINT('Origin',(-0.158771324027147,-0.275,0.));
#17915=CARTESIAN_POINT('',(-0.158771324027147,-0.275,0.));
#17916=CARTESIAN_POINT('',(0.158771324027147,-0.275,0.));
#17917=CARTESIAN_POINT('',(-0.158771324027147,-0.275,0.));
#17918=CARTESIAN_POINT('',(0.158771324027147,-0.275,0.));
#17919=CARTESIAN_POINT('',(-0.158771324027147,-0.275,0.));
#17920=CARTESIAN_POINT('Origin',(-0.317542648054294,3.88877587532466E-17,
0.));
#17921=CARTESIAN_POINT('',(-0.317542648054294,3.88877587532466E-17,0.));
#17922=CARTESIAN_POINT('',(-0.317542648054294,3.88877587532466E-17,0.));
#17923=CARTESIAN_POINT('',(-0.317542648054294,3.88877587532466E-17,0.));
#17924=CARTESIAN_POINT('Origin',(-0.158771324027147,0.275,0.));
#17925=CARTESIAN_POINT('',(-0.158771324027147,0.275,0.));
#17926=CARTESIAN_POINT('',(-0.158771324027147,0.275,0.));
#17927=CARTESIAN_POINT('',(-0.158771324027147,0.275,0.));
#17928=CARTESIAN_POINT('Origin',(0.158771324027147,0.275,0.));
#17929=CARTESIAN_POINT('',(0.158771324027147,0.275,0.));
#17930=CARTESIAN_POINT('',(0.158771324027147,0.275,0.));
#17931=CARTESIAN_POINT('',(0.158771324027147,0.275,0.));
#17932=CARTESIAN_POINT('Origin',(0.317542648054294,0.,0.));
#17933=CARTESIAN_POINT('',(0.317542648054294,0.,0.));
#17934=CARTESIAN_POINT('',(0.317542648054294,0.,0.));
#17935=CARTESIAN_POINT('',(0.317542648054294,0.,0.));
#17936=CARTESIAN_POINT('Origin',(0.158771324027147,-0.275,0.));
#17937=CARTESIAN_POINT('',(0.158771324027147,-0.275,0.));
#17938=CARTESIAN_POINT('Origin',(0.,0.,0.));
#17939=CARTESIAN_POINT('',(0.,0.,0.));
#17940=CARTESIAN_POINT('Origin',(2.,0.,1.));
#17941=CARTESIAN_POINT('',(1.65,4.28626379701574E-17,1.1));
#17942=CARTESIAN_POINT('Origin',(2.,0.,1.1));
#17943=CARTESIAN_POINT('',(1.65,4.28626379701574E-17,0.9));
#17944=CARTESIAN_POINT('',(1.65,4.28626379701574E-17,1.));
#17945=CARTESIAN_POINT('Origin',(2.,0.,0.9));
#17946=CARTESIAN_POINT('Origin',(8.8,0.,1.));
#17947=CARTESIAN_POINT('',(8.45,4.28626379701574E-17,1.1));
#17948=CARTESIAN_POINT('Origin',(8.8,0.,1.1));
#17949=CARTESIAN_POINT('',(8.45,4.28626379701574E-17,0.9));
#17950=CARTESIAN_POINT('',(8.45,4.28626379701574E-17,1.));
#17951=CARTESIAN_POINT('Origin',(8.8,0.,0.9));
#17952=CARTESIAN_POINT('Origin',(8.1,1.,0.7));
#17953=CARTESIAN_POINT('',(7.85,1.,0.7));
#17954=CARTESIAN_POINT('Origin',(8.1,1.,0.7));
#17955=CARTESIAN_POINT('',(7.95,1.,0.7));
#17956=CARTESIAN_POINT('Origin',(8.1,1.,0.7));
#17957=CARTESIAN_POINT('Origin',(8.1,1.,0.7));
#17958=CARTESIAN_POINT('',(7.85,1.,0.6));
#17959=CARTESIAN_POINT('Origin',(8.1,1.,0.6));
#17960=CARTESIAN_POINT('',(7.85,1.,0.7));
#17961=CARTESIAN_POINT('Origin',(8.1,1.,0.6));
#17962=CARTESIAN_POINT('Origin',(2.7,-1.,0.7));
#17963=CARTESIAN_POINT('',(2.45,-1.,0.7));
#17964=CARTESIAN_POINT('Origin',(2.7,-1.,0.7));
#17965=CARTESIAN_POINT('',(2.55,-1.,0.7));
#17966=CARTESIAN_POINT('Origin',(2.7,-1.,0.7));
#17967=CARTESIAN_POINT('Origin',(2.7,-1.,0.7));
#17968=CARTESIAN_POINT('',(2.45,-1.,0.6));
#17969=CARTESIAN_POINT('Origin',(2.7,-1.,0.6));
#17970=CARTESIAN_POINT('',(2.45,-1.,0.7));
#17971=CARTESIAN_POINT('Origin',(2.7,-1.,0.6));
#17972=CARTESIAN_POINT('Origin',(2.7,1.,0.7));
#17973=CARTESIAN_POINT('',(2.45,1.,0.7));
#17974=CARTESIAN_POINT('Origin',(2.7,1.,0.7));
#17975=CARTESIAN_POINT('',(2.55,1.,0.7));
#17976=CARTESIAN_POINT('Origin',(2.7,1.,0.7));
#17977=CARTESIAN_POINT('Origin',(2.7,1.,0.7));
#17978=CARTESIAN_POINT('',(2.45,1.,0.6));
#17979=CARTESIAN_POINT('Origin',(2.7,1.,0.6));
#17980=CARTESIAN_POINT('',(2.45,1.,0.7));
#17981=CARTESIAN_POINT('Origin',(2.7,1.,0.6));
#17982=CARTESIAN_POINT('Origin',(8.1,-1.,0.7));
#17983=CARTESIAN_POINT('',(7.85,-1.,0.7));
#17984=CARTESIAN_POINT('Origin',(8.1,-1.,0.7));
#17985=CARTESIAN_POINT('',(7.95,-1.,0.7));
#17986=CARTESIAN_POINT('Origin',(8.1,-1.,0.7));
#17987=CARTESIAN_POINT('Origin',(8.1,-1.,0.7));
#17988=CARTESIAN_POINT('',(7.85,-1.,0.6));
#17989=CARTESIAN_POINT('Origin',(8.1,-1.,0.6));
#17990=CARTESIAN_POINT('',(7.85,-1.,0.7));
#17991=CARTESIAN_POINT('Origin',(8.1,-1.,0.6));
#17992=CARTESIAN_POINT('Origin',(8.1,1.,0.9));
#17993=CARTESIAN_POINT('',(7.95,1.,0.9));
#17994=CARTESIAN_POINT('',(7.95,1.,0.9));
#17995=CARTESIAN_POINT('Origin',(8.1,1.,0.9));
#17996=CARTESIAN_POINT('Origin',(2.7,-1.,0.9));
#17997=CARTESIAN_POINT('',(2.55,-1.,0.9));
#17998=CARTESIAN_POINT('',(2.55,-1.,0.9));
#17999=CARTESIAN_POINT('Origin',(2.7,-1.,0.9));
#18000=CARTESIAN_POINT('Origin',(2.7,1.,0.9));
#18001=CARTESIAN_POINT('',(2.55,1.,0.9));
#18002=CARTESIAN_POINT('',(2.55,1.,0.9));
#18003=CARTESIAN_POINT('Origin',(2.7,1.,0.9));
#18004=CARTESIAN_POINT('Origin',(8.1,-1.,0.9));
#18005=CARTESIAN_POINT('',(7.95,-1.,0.9));
#18006=CARTESIAN_POINT('',(7.95,-1.,0.9));
#18007=CARTESIAN_POINT('Origin',(8.1,-1.,0.9));
#18008=CARTESIAN_POINT('Ctrl Pts',(10.3006295894369,0.974894988741159,1.1));
#18009=CARTESIAN_POINT('Ctrl Pts',(10.315705472156,0.974011521809381,1.1));
#18010=CARTESIAN_POINT('Ctrl Pts',(10.3502474882039,0.960160784532573,1.1));
#18011=CARTESIAN_POINT('Ctrl Pts',(10.3664342774515,0.92524659453289,1.1));
#18012=CARTESIAN_POINT('Ctrl Pts',(10.3664342774515,0.905110932257975,1.1));
#18013=CARTESIAN_POINT('Ctrl Pts',(10.3019806204244,0.997949597787003,1.1));
#18014=CARTESIAN_POINT('Ctrl Pts',(10.3220349090938,0.996609784625678,1.09999398337427));
#18015=CARTESIAN_POINT('Ctrl Pts',(10.3677183242066,0.978025516808524,1.09998506712737));
#18016=CARTESIAN_POINT('Ctrl Pts',(10.3893396302527,0.931918448901421,1.09999143472557));
#18017=CARTESIAN_POINT('Ctrl Pts',(10.3895723566779,0.905110932257975,1.1));
#18018=CARTESIAN_POINT('Ctrl Pts',(10.3043223099121,1.03790925537118,1.08136572286424));
#18019=CARTESIAN_POINT('Ctrl Pts',(10.3329503749445,1.0358015962555,1.08164234815929));
#18020=CARTESIAN_POINT('Ctrl Pts',(10.3979372989902,1.00899285190124,1.08203919297574));
#18021=CARTESIAN_POINT('Ctrl Pts',(10.4290660105163,0.943405843911333,1.08168333012239));
#18022=CARTESIAN_POINT('Ctrl Pts',(10.4296737498558,0.905110932257975,1.08129070628762));
#18023=CARTESIAN_POINT('Ctrl Pts',(10.3052465815697,1.05368144854439,1.04171131144128));
#18024=CARTESIAN_POINT('Ctrl Pts',(10.3373036016374,1.05157771141627,1.04242733672965));
#18025=CARTESIAN_POINT('Ctrl Pts',(10.4104769365187,1.02185126978705,1.04346621563788));
#18026=CARTESIAN_POINT('Ctrl Pts',(10.445100550936,0.94795146444073,1.04253150017828));
#18027=CARTESIAN_POINT('Ctrl Pts',(10.4454164251054,0.905110932257975,1.0415166534692));
#18028=CARTESIAN_POINT('Ctrl Pts',(10.3053025283406,1.05463614976313,1.02441711227736));
#18029=CARTESIAN_POINT('Ctrl Pts',(10.3375636805833,1.05269876817044,1.02526261130878));
#18030=CARTESIAN_POINT('Ctrl Pts',(10.411517621087,1.0229540574362,1.02649649899074));
#18031=CARTESIAN_POINT('Ctrl Pts',(10.4462618831994,0.948196125723061,1.02538435201347));
#18032=CARTESIAN_POINT('Ctrl Pts',(10.4463246402318,0.905110932257975,1.02418687649944));
#18033=CARTESIAN_POINT('',(10.3664342774515,0.905110932257975,1.1));
#18034=CARTESIAN_POINT('',(10.4463246402318,0.905110932257975,1.02418687649943));
#18035=CARTESIAN_POINT('Origin',(10.3664342774515,0.905110932257975,1.02));
#18036=CARTESIAN_POINT('',(10.3053025283406,1.05463614976313,1.02441711227738));
#18037=CARTESIAN_POINT('Ctrl Pts',(10.4463246402318,0.905110932257975,1.02418687649944));
#18038=CARTESIAN_POINT('Ctrl Pts',(10.4462618831994,0.948196125723061,1.02538435201347));
#18039=CARTESIAN_POINT('Ctrl Pts',(10.411517621087,1.0229540574362,1.02649649899074));
#18040=CARTESIAN_POINT('Ctrl Pts',(10.3375636805833,1.05269876817044,1.02526261130878));
#18041=CARTESIAN_POINT('Ctrl Pts',(10.3053025283406,1.05463614976313,1.02441711227736));
#18042=CARTESIAN_POINT('',(10.3006295894369,0.974894988741159,1.1));
#18043=CARTESIAN_POINT('Origin',(10.3006295894369,0.974894988741159,1.02));
#18044=CARTESIAN_POINT('Ctrl Pts',(10.3006295894369,0.974894988741159,1.1));
#18045=CARTESIAN_POINT('Ctrl Pts',(10.315705472156,0.974011521809381,1.1));
#18046=CARTESIAN_POINT('Ctrl Pts',(10.3502474882039,0.960160784532573,1.1));
#18047=CARTESIAN_POINT('Ctrl Pts',(10.3664342774515,0.92524659453289,1.1));
#18048=CARTESIAN_POINT('Ctrl Pts',(10.3664342774515,0.905110932257975,1.1));
#18049=CARTESIAN_POINT('Origin',(10.3664342774515,0.526416499322631,1.02));
#18050=CARTESIAN_POINT('',(10.3664342774515,-0.905110932257974,1.1));
#18051=CARTESIAN_POINT('',(10.4463246402318,-0.905110932257974,1.02418687649944));
#18052=CARTESIAN_POINT('Origin',(10.3664342774515,-0.905110932257974,1.02));
#18053=CARTESIAN_POINT('',(10.4463246402318,0.526416499322631,1.02418687649944));
#18054=CARTESIAN_POINT('',(10.3664342774515,0.526416499322631,1.1));
#18055=CARTESIAN_POINT('Ctrl Pts',(10.3664342774515,-0.905110932257974,
1.1));
#18056=CARTESIAN_POINT('Ctrl Pts',(10.3664342774515,-0.920212678972614,
1.1));
#18057=CARTESIAN_POINT('Ctrl Pts',(10.3546350195413,-0.955507038097987,
1.1));
#18058=CARTESIAN_POINT('Ctrl Pts',(10.3207307664069,-0.973717032831462,
1.1));
#18059=CARTESIAN_POINT('Ctrl Pts',(10.3006295894369,-0.974894988741159,
1.1));
#18060=CARTESIAN_POINT('Ctrl Pts',(10.3895723566779,-0.905110932257974,
1.1));
#18061=CARTESIAN_POINT('Ctrl Pts',(10.3893978118589,-0.925216569751813,
1.09999357604418));
#18062=CARTESIAN_POINT('Ctrl Pts',(10.3734893817427,-0.971910228734234,
1.09998467394719));
#18063=CARTESIAN_POINT('Ctrl Pts',(10.3287196719985,-0.996163180237569,
1.09999197783236));
#18064=CARTESIAN_POINT('Ctrl Pts',(10.3019806204244,-0.997949597787003,
1.1));
#18065=CARTESIAN_POINT('Ctrl Pts',(10.4296737498558,-0.905110932257974,
1.0812907062876));
#18066=CARTESIAN_POINT('Ctrl Pts',(10.4292179453509,-0.933832116014069,
1.08158517416384));
#18067=CARTESIAN_POINT('Ctrl Pts',(10.4061705706524,-1.00027633256302,1.08203447943735));
#18068=CARTESIAN_POINT('Ctrl Pts',(10.3424930633099,-1.03509904321534,1.08173455659116));
#18069=CARTESIAN_POINT('Ctrl Pts',(10.3043223099121,-1.03790925537115,1.08136572286421));
#18070=CARTESIAN_POINT('Ctrl Pts',(10.4454164251054,-0.905110932257974,
1.0415166534692));
#18071=CARTESIAN_POINT('Ctrl Pts',(10.4451795194782,-0.937241331413026,
1.04227778850144));
#18072=CARTESIAN_POINT('Ctrl Pts',(10.4197512278104,-1.01202259423409,1.0434534732467));
#18073=CARTESIAN_POINT('Ctrl Pts',(10.3479892750172,-1.05087646570533,1.0426660118263));
#18074=CARTESIAN_POINT('Ctrl Pts',(10.3052465815697,-1.05368144854438,1.04171131144128));
#18075=CARTESIAN_POINT('Ctrl Pts',(10.4463246402318,-0.905110932257974,
1.02418687649944));
#18076=CARTESIAN_POINT('Ctrl Pts',(10.4462775724575,-0.937424827374877,
1.02508498313546));
#18077=CARTESIAN_POINT('Ctrl Pts',(10.4209202812412,-1.01298254961426,1.02648109501254));
#18078=CARTESIAN_POINT('Ctrl Pts',(10.3483173980216,-1.05205297430477,1.02554444431988));
#18079=CARTESIAN_POINT('Ctrl Pts',(10.3053025283406,-1.05463614976313,1.02441711227736));
#18080=CARTESIAN_POINT('',(10.3006295894369,-0.974894988741159,1.1));
#18081=CARTESIAN_POINT('',(10.3053025283406,-1.05463614976313,1.02441711227736));
#18082=CARTESIAN_POINT('Origin',(10.3006295894369,-0.974894988741159,1.02));
#18083=CARTESIAN_POINT('Ctrl Pts',(10.3053025283406,-1.05463614976313,1.02441711227736));
#18084=CARTESIAN_POINT('Ctrl Pts',(10.3483173980216,-1.05205297430477,1.02554444431988));
#18085=CARTESIAN_POINT('Ctrl Pts',(10.4209202812412,-1.01298254961426,1.02648109501254));
#18086=CARTESIAN_POINT('Ctrl Pts',(10.4462775724575,-0.937424827374877,
1.02508498313546));
#18087=CARTESIAN_POINT('Ctrl Pts',(10.4463246402318,-0.905110932257974,
1.02418687649944));
#18088=CARTESIAN_POINT('Ctrl Pts',(10.3664342774515,-0.905110932257974,
1.1));
#18089=CARTESIAN_POINT('Ctrl Pts',(10.3664342774515,-0.920212678972614,
1.1));
#18090=CARTESIAN_POINT('Ctrl Pts',(10.3546350195413,-0.955507038097987,
1.1));
#18091=CARTESIAN_POINT('Ctrl Pts',(10.3207307664069,-0.973717032831462,
1.1));
#18092=CARTESIAN_POINT('Ctrl Pts',(10.3006295894369,-0.974894988741159,
1.1));
#18093=CARTESIAN_POINT('Ctrl Pts',(10.3006295894369,-0.974894988741159,
1.1));
#18094=CARTESIAN_POINT('Ctrl Pts',(8.90133038997308,-1.05689579714676,1.1));
#18095=CARTESIAN_POINT('Ctrl Pts',(5.63386529032775,-1.20659234980357,1.1));
#18096=CARTESIAN_POINT('Ctrl Pts',(2.35953432096223,-1.1387902266302,1.1));
#18097=CARTESIAN_POINT('Ctrl Pts',(0.497468741075922,-0.978719373910683,
1.1));
#18098=CARTESIAN_POINT('Ctrl Pts',(10.3019806204244,-0.997949597787003,
1.1));
#18099=CARTESIAN_POINT('Ctrl Pts',(8.90248440956766,-1.07998148241326,1.10000071389857));
#18100=CARTESIAN_POINT('Ctrl Pts',(5.63428345559727,-1.22975661509925,1.09999860206726));
#18101=CARTESIAN_POINT('Ctrl Pts',(2.35854977485598,-1.16192218645588,1.10000206853834));
#18102=CARTESIAN_POINT('Ctrl Pts',(0.495492436783665,-1.00170924455528,
1.1));
#18103=CARTESIAN_POINT('Ctrl Pts',(10.3043223112023,-1.03790927738781,1.08136574244164));
#18104=CARTESIAN_POINT('Ctrl Pts',(8.90448672538924,-1.11999254202045,1.08133291965814));
#18105=CARTESIAN_POINT('Ctrl Pts',(5.63501252140964,-1.26990499402305,1.08126385742935));
#18106=CARTESIAN_POINT('Ctrl Pts',(2.35683262246169,-1.20200947624765,1.08130376582018));
#18107=CARTESIAN_POINT('Ctrl Pts',(0.492066872450609,-1.0415580073244,1.08139899772624));
#18108=CARTESIAN_POINT('Ctrl Pts',(10.3052465815697,-1.05368144854439,1.04171131144128));
#18109=CARTESIAN_POINT('Ctrl Pts',(8.90527383415966,-1.13574844311122,1.04162635195479));
#18110=CARTESIAN_POINT('Ctrl Pts',(5.63529344743191,-1.28563363803111,1.04144655753461));
#18111=CARTESIAN_POINT('Ctrl Pts',(2.35616768559357,-1.21776439538312,1.04155103737704));
#18112=CARTESIAN_POINT('Ctrl Pts',(0.490711556403977,-1.05732407164794,
1.04179769276967));
#18113=CARTESIAN_POINT('Ctrl Pts',(10.3053025283406,-1.05463614976313,1.02441711227736));
#18114=CARTESIAN_POINT('Ctrl Pts',(8.90532084970199,-1.13668250951809,1.02431679017323));
#18115=CARTESIAN_POINT('Ctrl Pts',(5.63530902077156,-1.28652517622799,1.02410366945797));
#18116=CARTESIAN_POINT('Ctrl Pts',(2.35612886002319,-1.2186808487933,1.02422798328229));
#18117=CARTESIAN_POINT('Ctrl Pts',(0.490627822843887,-1.05829812393464,
1.02451933428366));
#18118=CARTESIAN_POINT('',(0.497468741075922,-0.978719373910683,1.1));
#18119=CARTESIAN_POINT('',(0.490627822843887,-1.05829812393464,1.02451933428366));
#18120=CARTESIAN_POINT('Origin',(0.497468741075922,-0.978719373910683,1.02));
#18121=CARTESIAN_POINT('Ctrl Pts',(0.490627822843887,-1.05829812393464,
1.02451933428366));
#18122=CARTESIAN_POINT('Ctrl Pts',(2.35612886002319,-1.2186808487933,1.02422798328229));
#18123=CARTESIAN_POINT('Ctrl Pts',(5.63530902077156,-1.28652517622799,1.02410366945797));
#18124=CARTESIAN_POINT('Ctrl Pts',(8.90532084970199,-1.13668250951809,1.02431679017323));
#18125=CARTESIAN_POINT('Ctrl Pts',(10.3053025283406,-1.05463614976313,1.02441711227736));
#18126=CARTESIAN_POINT('Ctrl Pts',(10.3006295894369,-0.974894988741159,
1.1));
#18127=CARTESIAN_POINT('Ctrl Pts',(8.90133038997308,-1.05689579714676,1.1));
#18128=CARTESIAN_POINT('Ctrl Pts',(5.63386529032775,-1.20659234980357,1.1));
#18129=CARTESIAN_POINT('Ctrl Pts',(2.35953432096223,-1.1387902266302,1.1));
#18130=CARTESIAN_POINT('Ctrl Pts',(0.497468741075922,-0.978719373910683,
1.1));
#18131=CARTESIAN_POINT('Ctrl Pts',(0.497468741075921,-0.978719373910683,
1.1));
#18132=CARTESIAN_POINT('Ctrl Pts',(0.482693827936028,-0.977449261315989,
1.1));
#18133=CARTESIAN_POINT('Ctrl Pts',(0.449140492346353,-0.963153189418853,
1.1));
#18134=CARTESIAN_POINT('Ctrl Pts',(0.433565722548535,-0.928845297374623,
1.1));
#18135=CARTESIAN_POINT('Ctrl Pts',(0.433565722548535,-0.909072757750428,
1.1));
#18136=CARTESIAN_POINT('Ctrl Pts',(0.495492436783665,-1.00170924455528,
1.1));
#18137=CARTESIAN_POINT('Ctrl Pts',(0.475845599502289,-0.99986336234735,
1.09999428725696));
#18138=CARTESIAN_POINT('Ctrl Pts',(0.431470670910625,-0.980707626108276,
1.09998595101222));
#18139=CARTESIAN_POINT('Ctrl Pts',(0.410656014536328,-0.935396857641307,
1.09999159501496));
#18140=CARTESIAN_POINT('Ctrl Pts',(0.410427643322096,-0.909072757750428,
1.1));
#18141=CARTESIAN_POINT('Ctrl Pts',(0.49206544526959,-1.04157460937658,1.08141381101793));
#18142=CARTESIAN_POINT('Ctrl Pts',(0.464027324938814,-1.03875422423143,
1.08167681576789));
#18143=CARTESIAN_POINT('Ctrl Pts',(0.40089609645214,-1.01114975683443,1.0820463630617));
#18144=CARTESIAN_POINT('Ctrl Pts',(0.370905720538455,-0.946677133941945,
1.08169093175476));
#18145=CARTESIAN_POINT('Ctrl Pts',(0.370309354350992,-0.909072757750428,
1.08130565542949));
#18146=CARTESIAN_POINT('Ctrl Pts',(0.490711556403977,-1.05732407164794,
1.04179769276967));
#18147=CARTESIAN_POINT('Ctrl Pts',(0.459302109313527,-1.05440855600651,
1.04247888820671));
#18148=CARTESIAN_POINT('Ctrl Pts',(0.388222412631637,-1.02376232464153,
1.04344633806995));
#18149=CARTESIAN_POINT('Ctrl Pts',(0.354893537837358,-0.951140796546497,
1.04251250847383));
#18150=CARTESIAN_POINT('Ctrl Pts',(0.354583574894625,-0.909072757750428,
1.0415166534692));
#18151=CARTESIAN_POINT('Ctrl Pts',(0.490627822843887,-1.05829812393464,
1.02451933428366));
#18152=CARTESIAN_POINT('Ctrl Pts',(0.45900946369528,-1.05553438344805,1.02532396689517));
#18153=CARTESIAN_POINT('Ctrl Pts',(0.387169680965019,-1.0248398620393,1.02647307310763));
#18154=CARTESIAN_POINT('Ctrl Pts',(0.353736942373964,-0.951381046565093,
1.02536194261819));
#18155=CARTESIAN_POINT('Ctrl Pts',(0.35367535976817,-0.909072757750428,
1.02418687649944));
#18156=CARTESIAN_POINT('',(0.433565722548535,-0.909072757750428,1.1));
#18157=CARTESIAN_POINT('',(0.35367535976817,-0.909072757750428,1.02418687649944));
#18158=CARTESIAN_POINT('Origin',(0.433565722548536,-0.909072757750428,1.02));
#18159=CARTESIAN_POINT('Ctrl Pts',(0.35367535976817,-0.909072757750428,
1.02418687649944));
#18160=CARTESIAN_POINT('Ctrl Pts',(0.353736942373964,-0.951381046565093,
1.02536194261819));
#18161=CARTESIAN_POINT('Ctrl Pts',(0.387169680965019,-1.0248398620393,1.02647307310763));
#18162=CARTESIAN_POINT('Ctrl Pts',(0.45900946369528,-1.05553438344805,1.02532396689517));
#18163=CARTESIAN_POINT('Ctrl Pts',(0.490627822843887,-1.05829812393464,
1.02451933428366));
#18164=CARTESIAN_POINT('Ctrl Pts',(0.497468741075921,-0.978719373910683,
1.1));
#18165=CARTESIAN_POINT('Ctrl Pts',(0.482693827936028,-0.977449261315989,
1.1));
#18166=CARTESIAN_POINT('Ctrl Pts',(0.449140492346353,-0.963153189418853,
1.1));
#18167=CARTESIAN_POINT('Ctrl Pts',(0.433565722548535,-0.928845297374623,
1.1));
#18168=CARTESIAN_POINT('Ctrl Pts',(0.433565722548535,-0.909072757750428,
1.1));
#18169=CARTESIAN_POINT('Origin',(0.433565722548535,-0.526416499322631,1.02));
#18170=CARTESIAN_POINT('',(0.433565722548535,0.909072757750428,1.1));
#18171=CARTESIAN_POINT('',(0.35367535976817,0.909072757750428,1.02418687649944));
#18172=CARTESIAN_POINT('Origin',(0.433565722548535,0.909072757750428,1.02));
#18173=CARTESIAN_POINT('',(0.35367535976817,-0.526416499322631,1.02418687649944));
#18174=CARTESIAN_POINT('',(0.433565722548535,-0.526416499322631,1.1));
#18175=CARTESIAN_POINT('Ctrl Pts',(0.433565722548535,0.909072757750428,
1.1));
#18176=CARTESIAN_POINT('Ctrl Pts',(0.433565722548535,0.923902162481473,
1.1));
#18177=CARTESIAN_POINT('Ctrl Pts',(0.444925688709976,0.95855828847753,1.1));
#18178=CARTESIAN_POINT('Ctrl Pts',(0.477768856872262,0.977025890449618,
1.1));
#18179=CARTESIAN_POINT('Ctrl Pts',(0.497468741075921,0.978719373910683,
1.1));
#18180=CARTESIAN_POINT('Ctrl Pts',(0.410427643322096,0.909072757750428,
1.1));
#18181=CARTESIAN_POINT('Ctrl Pts',(0.410598921732919,0.928815832685761,
1.09999369626122));
#18182=CARTESIAN_POINT('Ctrl Pts',(0.425924740546693,0.974670094016788,
1.09998538828789));
#18183=CARTESIAN_POINT('Ctrl Pts',(0.469296653719045,0.9992480682759,1.09999238300928));
#18184=CARTESIAN_POINT('Ctrl Pts',(0.495492436783665,1.00170924455528,1.1));
#18185=CARTESIAN_POINT('Ctrl Pts',(0.370309354350991,0.909072757750428,
1.08130565542949));
#18186=CARTESIAN_POINT('Ctrl Pts',(0.370756628991978,0.937276039918598,
1.0815946126737));
#18187=CARTESIAN_POINT('Ctrl Pts',(0.392976709797646,1.00253976529927,1.08203966084696));
#18188=CARTESIAN_POINT('Ctrl Pts',(0.454681284796039,1.03781409584644,1.08176448401818));
#18189=CARTESIAN_POINT('Ctrl Pts',(0.49206544526959,1.04157460937658,1.08141381101793));
#18190=CARTESIAN_POINT('Ctrl Pts',(0.354583574894625,0.909072757750428,
1.0415166534692));
#18191=CARTESIAN_POINT('Ctrl Pts',(0.354816047101877,0.940623786874923,
1.04226354472332));
#18192=CARTESIAN_POINT('Ctrl Pts',(0.379310481833935,1.01405872099116,1.04342813304911));
#18193=CARTESIAN_POINT('Ctrl Pts',(0.448832293580284,1.05343671745598,1.04270595335318));
#18194=CARTESIAN_POINT('Ctrl Pts',(0.490711556403977,1.05732407164794,1.04179769276967));
#18195=CARTESIAN_POINT('Ctrl Pts',(0.35367535976817,0.909072757750428,1.02418687649944));
#18196=CARTESIAN_POINT('Ctrl Pts',(0.353721546722556,0.940803974389028,
1.02506817608927));
#18197=CARTESIAN_POINT('Ctrl Pts',(0.378136805744942,1.01499479618886,1.02645106984513));
#18198=CARTESIAN_POINT('Ctrl Pts',(0.448470010609076,1.05461313661598,1.0255921777666));
#18199=CARTESIAN_POINT('Ctrl Pts',(0.490627822843887,1.05829812393464,1.02451933428366));
#18200=CARTESIAN_POINT('',(0.497468741075921,0.978719373910683,1.1));
#18201=CARTESIAN_POINT('',(0.490627822843887,1.05829812393464,1.02451933428366));
#18202=CARTESIAN_POINT('Origin',(0.497468741075921,0.978719373910683,1.02));
#18203=CARTESIAN_POINT('Ctrl Pts',(0.490627822843887,1.05829812393464,1.02451933428366));
#18204=CARTESIAN_POINT('Ctrl Pts',(0.448470010609076,1.05461313661598,1.0255921777666));
#18205=CARTESIAN_POINT('Ctrl Pts',(0.378136805744942,1.01499479618886,1.02645106984513));
#18206=CARTESIAN_POINT('Ctrl Pts',(0.353721546722556,0.940803974389028,
1.02506817608927));
#18207=CARTESIAN_POINT('Ctrl Pts',(0.35367535976817,0.909072757750428,1.02418687649944));
#18208=CARTESIAN_POINT('Ctrl Pts',(0.433565722548535,0.909072757750428,
1.1));
#18209=CARTESIAN_POINT('Ctrl Pts',(0.433565722548535,0.923902162481473,
1.1));
#18210=CARTESIAN_POINT('Ctrl Pts',(0.444925688709976,0.95855828847753,1.1));
#18211=CARTESIAN_POINT('Ctrl Pts',(0.477768856872262,0.977025890449618,
1.1));
#18212=CARTESIAN_POINT('Ctrl Pts',(0.497468741075921,0.978719373910683,
1.1));
#18213=CARTESIAN_POINT('Ctrl Pts',(0.497468741075922,0.978719373910683,
1.1));
#18214=CARTESIAN_POINT('Ctrl Pts',(1.89401780684616,1.09877250320817,1.1));
#18215=CARTESIAN_POINT('Ctrl Pts',(5.1654052076905,1.21987569230965,1.1));
#18216=CARTESIAN_POINT('Ctrl Pts',(8.43489748265729,1.08422939062092,1.1));
#18217=CARTESIAN_POINT('Ctrl Pts',(10.3006295894369,0.974894988741159,1.1));
#18218=CARTESIAN_POINT('Ctrl Pts',(0.495492436783665,1.00170924455528,1.1));
#18219=CARTESIAN_POINT('Ctrl Pts',(1.89278532112995,1.12186894072949,1.10000155140362));
#18220=CARTESIAN_POINT('Ctrl Pts',(5.16566149651331,1.24305592512388,1.09999870932828));
#18221=CARTESIAN_POINT('Ctrl Pts',(8.43598583180997,1.1073254346241,1.10000095186468));
#18222=CARTESIAN_POINT('Ctrl Pts',(10.3019806204244,0.997949597787003,1.1));
#18223=CARTESIAN_POINT('Ctrl Pts',(0.492066872450609,1.0415580073244,1.08139899772624));
#18224=CARTESIAN_POINT('Ctrl Pts',(1.89064106564166,1.16189659875033,1.08132757380279));
#18225=CARTESIAN_POINT('Ctrl Pts',(5.16610832342906,1.28323142649893,1.0812556832418));
#18226=CARTESIAN_POINT('Ctrl Pts',(8.43787502268472,1.14735362089424,1.08132197873404));
#18227=CARTESIAN_POINT('Ctrl Pts',(10.3043223112023,1.03790927738781,1.08136574244164));
#18228=CARTESIAN_POINT('Ctrl Pts',(0.490711556403977,1.05732407164794,1.04179769276967));
#18229=CARTESIAN_POINT('Ctrl Pts',(1.88980353393473,1.17765430418353,1.04161270124098));
#18230=CARTESIAN_POINT('Ctrl Pts',(5.16628155123749,1.29896165650174,1.04142536433641));
#18231=CARTESIAN_POINT('Ctrl Pts',(8.43861641093843,1.16310409863161,1.04159803213562));
#18232=CARTESIAN_POINT('Ctrl Pts',(10.3052465815697,1.05368144854439,1.04171131144128));
#18233=CARTESIAN_POINT('Ctrl Pts',(0.490627822843887,1.05829812393464,1.02451933428366));
#18234=CARTESIAN_POINT('Ctrl Pts',(1.88975348136405,1.17858515731652,1.02430082105127));
#18235=CARTESIAN_POINT('Ctrl Pts',(5.16629169073646,1.29984841142479,1.02407861909595));
#18236=CARTESIAN_POINT('Ctrl Pts',(8.43866044940558,1.1640312867702,1.02428334948326));
#18237=CARTESIAN_POINT('Ctrl Pts',(10.3053025283406,1.05463614976313,1.02441711227736));
#18238=CARTESIAN_POINT('Ctrl Pts',(10.3053025283406,1.05463614976313,1.02441711227736));
#18239=CARTESIAN_POINT('Ctrl Pts',(8.43866044940558,1.1640312867702,1.02428334948326));
#18240=CARTESIAN_POINT('Ctrl Pts',(5.16629169073646,1.29984841142479,1.02407861909595));
#18241=CARTESIAN_POINT('Ctrl Pts',(1.88975348136405,1.17858515731652,1.02430082105127));
#18242=CARTESIAN_POINT('Ctrl Pts',(0.490627822843887,1.05829812393464,1.02451933428366));
#18243=CARTESIAN_POINT('Ctrl Pts',(0.497468741075922,0.978719373910683,
1.1));
#18244=CARTESIAN_POINT('Ctrl Pts',(1.89401780684616,1.09877250320817,1.1));
#18245=CARTESIAN_POINT('Ctrl Pts',(5.1654052076905,1.21987569230965,1.1));
#18246=CARTESIAN_POINT('Ctrl Pts',(8.43489748265729,1.08422939062092,1.1));
#18247=CARTESIAN_POINT('Ctrl Pts',(10.3006295894369,0.974894988741159,1.1));
#18248=CARTESIAN_POINT('Origin',(0.347167001354737,-1.05283299864526,0.9));
#18249=CARTESIAN_POINT('',(0.347167001354737,0.915565952400859,0.9));
#18250=CARTESIAN_POINT('Ctrl Pts',(0.347167001354737,0.915565952400859,
0.9));
#18251=CARTESIAN_POINT('Ctrl Pts',(0.349336454142569,0.913401548092598,
0.941395625182189));
#18252=CARTESIAN_POINT('Ctrl Pts',(0.351505906947026,0.911237149868421,
0.982791250681617));
#18253=CARTESIAN_POINT('Ctrl Pts',(0.35367535976817,0.909072757750428,1.02418687649944));
#18254=CARTESIAN_POINT('',(0.347167001354737,-0.915565952400859,0.9));
#18255=CARTESIAN_POINT('',(0.347167001354737,-1.05283299864526,0.9));
#18256=CARTESIAN_POINT('Ctrl Pts',(0.35367535976817,-0.909072757750428,
1.02418687649944));
#18257=CARTESIAN_POINT('Ctrl Pts',(0.351505906947026,-0.911237149868421,
0.982791250681617));
#18258=CARTESIAN_POINT('Ctrl Pts',(0.349336454142569,-0.913401548092598,
0.941395625182188));
#18259=CARTESIAN_POINT('Ctrl Pts',(0.347167001354737,-0.915565952400859,
0.9));
#18260=CARTESIAN_POINT('Ctrl Pts',(0.346993933238254,0.915738617787778,
0.896697663613103));
#18261=CARTESIAN_POINT('Ctrl Pts',(0.349221075397351,0.913516658022686,
0.939194067573829));
#18262=CARTESIAN_POINT('Ctrl Pts',(0.351448217573968,0.911294704668933,
0.981690471868858));
#18263=CARTESIAN_POINT('Ctrl Pts',(0.35367535976817,0.909072757750428,1.02418687649944));
#18264=CARTESIAN_POINT('Ctrl Pts',(0.3471095194732,0.958036394339727,0.898903180361322));
#18265=CARTESIAN_POINT('Ctrl Pts',(0.349336694827029,0.955813381999015,
0.941399523267081));
#18266=CARTESIAN_POINT('Ctrl Pts',(0.351563761373338,0.953590428181058,
0.983895874971514));
#18267=CARTESIAN_POINT('Ctrl Pts',(0.353790936839104,0.951367426011707,
1.0263922183879));
#18268=CARTESIAN_POINT('Ctrl Pts',(0.38058410360499,1.03143776743275,0.900986703480571));
#18269=CARTESIAN_POINT('Ctrl Pts',(0.382809509257377,1.02921304595835,0.943483042387942));
#18270=CARTESIAN_POINT('Ctrl Pts',(0.38503494445329,1.0269883029847,0.985979378580875));
#18271=CARTESIAN_POINT('Ctrl Pts',(0.38726034587086,1.02476358729949,1.02847571797107));
#18272=CARTESIAN_POINT('Ctrl Pts',(0.452370958194108,1.06215086202928,0.898830373501354));
#18273=CARTESIAN_POINT('Ctrl Pts',(0.454593549384999,1.0599273359084,0.941326919294252));
#18274=CARTESIAN_POINT('Ctrl Pts',(0.456816159498039,1.05770384366995,0.983823465869045));
#18275=CARTESIAN_POINT('Ctrl Pts',(0.459038739297573,1.0554803259981,1.02632001264655));
#18276=CARTESIAN_POINT('Ctrl Pts',(0.48397786901498,1.06495020962439,0.897320291708494));
#18277=CARTESIAN_POINT('Ctrl Pts',(0.486199596570706,1.06272777115298,0.939816939358577));
#18278=CARTESIAN_POINT('Ctrl Pts',(0.488421317286976,1.06050533819043,0.982313587627294));
#18279=CARTESIAN_POINT('Ctrl Pts',(0.49064303113777,1.05828291075608,1.02481023651688));
#18280=CARTESIAN_POINT('',(0.484117964332956,1.06481006947648,0.9));
#18281=CARTESIAN_POINT('Ctrl Pts',(0.490627822843887,1.05829812393464,1.02451933428366));
#18282=CARTESIAN_POINT('Ctrl Pts',(0.488457876548035,1.06046876718106,0.983012888930867));
#18283=CARTESIAN_POINT('Ctrl Pts',(0.486287923702977,1.06263941570101,0.941506444170341));
#18284=CARTESIAN_POINT('Ctrl Pts',(0.484117964332956,1.06481006947648,0.9));
#18285=CARTESIAN_POINT('Ctrl Pts',(0.484117964332956,1.06481006947648,0.9));
#18286=CARTESIAN_POINT('Ctrl Pts',(0.473400395954556,1.06388989254567,0.899999999998067));
#18287=CARTESIAN_POINT('Ctrl Pts',(0.462835544435656,1.06178983909504,0.899998456484708));
#18288=CARTESIAN_POINT('Ctrl Pts',(0.452598733053303,1.05860868771556,0.899998088469989));
#18289=CARTESIAN_POINT('Ctrl Pts',(0.444242646677269,1.05601198306707,0.899997788067582));
#18290=CARTESIAN_POINT('Ctrl Pts',(0.436104524303727,1.05269365102958,0.899998236040192));
#18291=CARTESIAN_POINT('Ctrl Pts',(0.428287607266336,1.04868302953039,0.899999222960128));
#18292=CARTESIAN_POINT('Ctrl Pts',(0.418720381516706,1.0437743780639,0.900000430864189));
#18293=CARTESIAN_POINT('Ctrl Pts',(0.409734998843702,1.03788190267505,0.900002558923036));
#18294=CARTESIAN_POINT('Ctrl Pts',(0.401509364000825,1.03108161209803,0.900001877425249));
#18295=CARTESIAN_POINT('Ctrl Pts',(0.400282968007853,1.0300677269361,0.900001775817754));
#18296=CARTESIAN_POINT('Ctrl Pts',(0.399073506836177,1.02903357975146,0.900001605039306));
#18297=CARTESIAN_POINT('Ctrl Pts',(0.397881626738084,1.02797933950107,0.900001345423406));
#18298=CARTESIAN_POINT('Ctrl Pts',(0.39256805719391,1.02327938780652,0.900000188019117));
#18299=CARTESIAN_POINT('Ctrl Pts',(0.387603264903844,1.01818054769329,0.899997323013939));
#18300=CARTESIAN_POINT('Ctrl Pts',(0.383010638913681,1.01272978836618,0.899994456107983));
#18301=CARTESIAN_POINT('Ctrl Pts',(0.37606924632558,1.00449139480359,0.899990123005355));
#18302=CARTESIAN_POINT('Ctrl Pts',(0.370046554889952,0.995534526609835,
0.899986018340436));
#18303=CARTESIAN_POINT('Ctrl Pts',(0.3650033874046,0.986038739193365,0.899984773108821));
#18304=CARTESIAN_POINT('Ctrl Pts',(0.361794276996282,0.979996300523246,
0.899983980732651));
#18305=CARTESIAN_POINT('Ctrl Pts',(0.358982518390177,0.973734765189587,
0.899984261914926));
#18306=CARTESIAN_POINT('Ctrl Pts',(0.356593362150852,0.967295151176304,
0.899985518247832));
#18307=CARTESIAN_POINT('Ctrl Pts',(0.352862932284158,0.957240334312622,
0.899987479886722));
#18308=CARTESIAN_POINT('Ctrl Pts',(0.350196128254646,0.946848238515865,
0.899991935314924));
#18309=CARTESIAN_POINT('Ctrl Pts',(0.348668140386249,0.936282377262574,
0.899995621109591));
#18310=CARTESIAN_POINT('Ctrl Pts',(0.347678076093379,0.929436195976283,
0.89999800933123));
#18311=CARTESIAN_POINT('Ctrl Pts',(0.347167001781036,0.922516504287414,
0.899999999966543));
#18312=CARTESIAN_POINT('Ctrl Pts',(0.347167001354737,0.915565952400859,
0.9));
#18313=CARTESIAN_POINT('Ctrl Pts',(0.484117964332956,1.06481006947648,0.9));
#18314=CARTESIAN_POINT('Ctrl Pts',(0.486234267105876,1.06263480888061,0.94150644476122));
#18315=CARTESIAN_POINT('Ctrl Pts',(0.488350569878795,1.06045954828474,0.98301288952244));
#18316=CARTESIAN_POINT('Ctrl Pts',(0.490466872651714,1.05828428768887,1.02451933428366));
#18317=CARTESIAN_POINT('Ctrl Pts',(3.76001591476243,1.34606837492147,0.9));
#18318=CARTESIAN_POINT('Ctrl Pts',(3.76072193310094,1.3438931143256,0.94150644476122));
#18319=CARTESIAN_POINT('Ctrl Pts',(3.76142795143945,1.34171785372973,0.98301288952244));
#18320=CARTESIAN_POINT('Ctrl Pts',(3.76213396977796,1.33954259313386,1.02451933428366));
#18321=CARTESIAN_POINT('Ctrl Pts',(7.03591386519191,1.25287427294368,0.9));
#18322=CARTESIAN_POINT('Ctrl Pts',(7.03520959909601,1.25069901234781,0.94150644476122));
#18323=CARTESIAN_POINT('Ctrl Pts',(7.03450533300011,1.24852375175194,0.98301288952244));
#18324=CARTESIAN_POINT('Ctrl Pts',(7.03380106690421,1.24634849115607,1.02451933428366));
#18325=CARTESIAN_POINT('Ctrl Pts',(10.3118118156214,1.06114656258054,0.9));
#18326=CARTESIAN_POINT('Ctrl Pts',(10.3096972650911,1.05897130198467,0.94150644476122));
#18327=CARTESIAN_POINT('Ctrl Pts',(10.3075827145608,1.0567960413888,0.98301288952244));
#18328=CARTESIAN_POINT('Ctrl Pts',(10.3054681640305,1.05462078079293,1.02451933428366));
#18329=CARTESIAN_POINT('',(10.3118118156214,1.06114656258054,0.9));
#18330=CARTESIAN_POINT('Ctrl Pts',(10.3118118156214,1.06114656258054,0.9));
#18331=CARTESIAN_POINT('Ctrl Pts',(10.3096420485163,1.05897642099582,0.941472370325488));
#18332=CARTESIAN_POINT('Ctrl Pts',(10.3074722860834,1.05680628338526,0.982944741084089));
#18333=CARTESIAN_POINT('Ctrl Pts',(10.3053025283406,1.05463614976313,1.02441711227738));
#18334=CARTESIAN_POINT('Ctrl Pts',(0.484117964332956,1.06481006947648,0.9));
#18335=CARTESIAN_POINT('Ctrl Pts',(3.76001591476244,1.34606837492147,0.9));
#18336=CARTESIAN_POINT('Ctrl Pts',(7.03591386519191,1.25287427294368,0.9));
#18337=CARTESIAN_POINT('Ctrl Pts',(10.3118118156214,1.06114656258054,0.9));
#18338=CARTESIAN_POINT('Ctrl Pts',(10.3119584735067,1.0612932457764,0.897196819041737));
#18339=CARTESIAN_POINT('Ctrl Pts',(10.3097363069231,1.05907069570186,0.939670735378922));
#18340=CARTESIAN_POINT('Ctrl Pts',(10.3075141452397,1.0568481497954,0.982144652170355));
#18341=CARTESIAN_POINT('Ctrl Pts',(10.3052919884757,1.05462560807237,1.02461856941773));
#18342=CARTESIAN_POINT('Ctrl Pts',(10.3549577591382,1.05865952187103,0.899312513938921));
#18343=CARTESIAN_POINT('Ctrl Pts',(10.3527348026837,1.05643589667682,0.941786332790264));
#18344=CARTESIAN_POINT('Ctrl Pts',(10.3505118643323,1.05421236578444,0.984260157591605));
#18345=CARTESIAN_POINT('Ctrl Pts',(10.348288915563,1.05198874626302,1.02673397710222));
#18346=CARTESIAN_POINT('Ctrl Pts',(10.427476572305,1.0195555601276,0.90106705940868));
#18347=CARTESIAN_POINT('Ctrl Pts',(10.4252515051274,1.01733143721131,0.943540744474557));
#18348=CARTESIAN_POINT('Ctrl Pts',(10.423026434404,1.01510729429004,0.986014428272043));
#18349=CARTESIAN_POINT('Ctrl Pts',(10.4208013694594,1.01288317591826,1.02848811366363));
#18350=CARTESIAN_POINT('Ctrl Pts',(10.452914163627,0.944082648463888,0.89845127988914));
#18351=CARTESIAN_POINT('Ctrl Pts',(10.4506882024692,0.941859792143813,0.940924989850352));
#18352=CARTESIAN_POINT('Ctrl Pts',(10.4484622663099,0.939636927142988,0.983398700650476));
#18353=CARTESIAN_POINT('Ctrl Pts',(10.4462363051112,0.937414078664829,1.02587241101113));
#18354=CARTESIAN_POINT('Ctrl Pts',(10.453002503567,0.911777874403687,0.896765653419433));
#18355=CARTESIAN_POINT('Ctrl Pts',(10.4507765491346,0.909555555737009,0.939239394205133));
#18356=CARTESIAN_POINT('Ctrl Pts',(10.4485505946895,0.90733324168256,0.981713135231494));
#18357=CARTESIAN_POINT('Ctrl Pts',(10.4463246402318,0.905110932257975,1.02418687649944));
#18358=CARTESIAN_POINT('',(10.4528329986453,0.911608646352005,0.9));
#18359=CARTESIAN_POINT('Ctrl Pts',(10.4463246402318,0.905110932257975,1.02418687649944));
#18360=CARTESIAN_POINT('Ctrl Pts',(10.4484940930483,0.90727683256362,0.982791250770435));
#18361=CARTESIAN_POINT('Ctrl Pts',(10.4506635458528,0.909442737267073,0.941395625270907));
#18362=CARTESIAN_POINT('Ctrl Pts',(10.4528329986453,0.911608646352005,0.9));
#18363=CARTESIAN_POINT('Ctrl Pts',(10.4528329986453,0.911608646352005,0.9));
#18364=CARTESIAN_POINT('Ctrl Pts',(10.4528329984504,0.922365992175136,0.899999999995018));
#18365=CARTESIAN_POINT('Ctrl Pts',(10.4516419184466,0.933071221555305,0.899998396191737));
#18366=CARTESIAN_POINT('Ctrl Pts',(10.4493455883239,0.943542152407774,0.899997878793429));
#18367=CARTESIAN_POINT('Ctrl Pts',(10.4474685729764,0.952101068966945,0.899997455873155));
#18368=CARTESIAN_POINT('Ctrl Pts',(10.4448518647823,0.96050416098414,0.899997731911133));
#18369=CARTESIAN_POINT('Ctrl Pts',(10.4415172538375,0.968646108261598,0.899998556768105));
#18370=CARTESIAN_POINT('Ctrl Pts',(10.4374420364703,0.978596355981088,0.899999564823172));
#18371=CARTESIAN_POINT('Ctrl Pts',(10.4323389624922,0.988051909949456,0.900001510869465));
#18372=CARTESIAN_POINT('Ctrl Pts',(10.4262707314398,0.996829854811629,0.900000879982417));
#18373=CARTESIAN_POINT('Ctrl Pts',(10.4250393574459,0.998611087749148,0.900000751961929));
#18374=CARTESIAN_POINT('Ctrl Pts',(10.4237680854757,1.0003643483506,0.900000505994341));
#18375=CARTESIAN_POINT('Ctrl Pts',(10.4224572101159,1.00208797543426,0.90000009374416));
#18376=CARTESIAN_POINT('Ctrl Pts',(10.4185057422955,1.00728363107359,0.899998851068177));
#18377=CARTESIAN_POINT('Ctrl Pts',(10.4141947510749,1.0122104380758,0.899996136506224));
#18378=CARTESIAN_POINT('Ctrl Pts',(10.4095592300387,1.01684760353016,0.899993329936423));
#18379=CARTESIAN_POINT('Ctrl Pts',(10.4019420261375,1.02446750958049,0.899988718110854));
#18380=CARTESIAN_POINT('Ctrl Pts',(10.3935294957569,1.03122853977634,0.899984126639313));
#18381=CARTESIAN_POINT('Ctrl Pts',(10.3844977038391,1.03705893037027,0.899982514537369));
#18382=CARTESIAN_POINT('Ctrl Pts',(10.3781912117148,1.04113002863034,0.899981388879436));
#18383=CARTESIAN_POINT('Ctrl Pts',(10.3715817027072,1.04474676663118,0.899981626398985));
#18384=CARTESIAN_POINT('Ctrl Pts',(10.364720849853,1.04787222446317,0.899983147799038));
#18385=CARTESIAN_POINT('Ctrl Pts',(10.3549611185069,1.05231826483487,0.899985312027903));
#18386=CARTESIAN_POINT('Ctrl Pts',(10.34479058664,1.05572789097839,0.899990169054599));
#18387=CARTESIAN_POINT('Ctrl Pts',(10.3343672593286,1.0580160164031,0.899994394012168));
#18388=CARTESIAN_POINT('Ctrl Pts',(10.3269595157814,1.05964216185967,0.899997396642827));
#18389=CARTESIAN_POINT('Ctrl Pts',(10.3194233385871,1.06070108442786,0.899999999979614));
#18390=CARTESIAN_POINT('Ctrl Pts',(10.3118118156214,1.06114656258054,0.9));
#18391=CARTESIAN_POINT('Origin',(5.4,6.06940689584926E-17,1.1));
#18392=CARTESIAN_POINT('Origin',(10.4528329986453,1.05283299864526,0.9));
#18393=CARTESIAN_POINT('',(10.4528329986453,-0.911608646352005,0.9));
#18394=CARTESIAN_POINT('Ctrl Pts',(10.4528329986453,-0.911608646352005,
0.9));
#18395=CARTESIAN_POINT('Ctrl Pts',(10.4506635458528,-0.909442737267072,
0.941395625270908));
#18396=CARTESIAN_POINT('Ctrl Pts',(10.4484940930483,-0.90727683256362,0.982791250770435));
#18397=CARTESIAN_POINT('Ctrl Pts',(10.4463246402318,-0.905110932257974,
1.02418687649944));
#18398=CARTESIAN_POINT('',(10.4528329986453,1.05283299864526,0.9));
#18399=CARTESIAN_POINT('Ctrl Pts',(0.483981659460312,-1.06494641796617,
0.897392794396587));
#18400=CARTESIAN_POINT('Ctrl Pts',(0.486202123526484,-1.0627252433871,0.939865274484676));
#18401=CARTESIAN_POINT('Ctrl Pts',(0.488422580760962,-1.06050407431064,
0.982337755190696));
#18402=CARTESIAN_POINT('Ctrl Pts',(0.49064303113777,-1.05828291075608,1.02481023651688));
#18403=CARTESIAN_POINT('Ctrl Pts',(0.441839113682364,-1.06121395205434,
0.899406236555586));
#18404=CARTESIAN_POINT('Ctrl Pts',(0.444060746976072,-1.05899130022525,
0.941878578466899));
#18405=CARTESIAN_POINT('Ctrl Pts',(0.446282352620465,-1.05676877539366,
0.984350928552248));
#18406=CARTESIAN_POINT('Ctrl Pts',(0.448503975350841,-1.05454613107877,
1.02682327135645));
#18407=CARTESIAN_POINT('Ctrl Pts',(0.371552730979752,-1.02159229167772,
0.901018138383736));
#18408=CARTESIAN_POINT('Ctrl Pts',(0.373777362914204,-1.01936901231721,
0.943490294374253));
#18409=CARTESIAN_POINT('Ctrl Pts',(0.376002007910301,-1.01714569791452,
0.985962447794501));
#18410=CARTESIAN_POINT('Ctrl Pts',(0.378226636819208,-1.01492242480963,
1.02843460423251));
#18411=CARTESIAN_POINT('Ctrl Pts',(0.347084422593646,-0.947458158036175,
0.898424303372123));
#18412=CARTESIAN_POINT('Ctrl Pts',(0.349310306978605,-0.945236691937326,
0.940896495998715));
#18413=CARTESIAN_POINT('Ctrl Pts',(0.351536158132471,-0.943015214174121,
0.983368689735046));
#18414=CARTESIAN_POINT('Ctrl Pts',(0.353762042571371,-0.940793758946387,
1.02584088291578));
#18415=CARTESIAN_POINT('Ctrl Pts',(0.346997732921341,-0.915734826946278,
0.896770165885443));
#18416=CARTESIAN_POINT('Ctrl Pts',(0.349223608519428,-0.913514130802309,
0.939242402422435));
#18417=CARTESIAN_POINT('Ctrl Pts',(0.351449484135017,-0.911293441062403,
0.981714639293352));
#18418=CARTESIAN_POINT('Ctrl Pts',(0.35367535976817,-0.909072757750428,
1.02418687649944));
#18419=CARTESIAN_POINT('',(0.484117964332957,-1.06481006947648,0.9));
#18420=CARTESIAN_POINT('Ctrl Pts',(0.347167001354737,-0.915565952400859,
0.9));
#18421=CARTESIAN_POINT('Ctrl Pts',(0.347167001618251,-0.926324952789844,
0.899999999993398));
#18422=CARTESIAN_POINT('Ctrl Pts',(0.348355267190738,-0.937032860435638,
0.899998616841383));
#18423=CARTESIAN_POINT('Ctrl Pts',(0.350648507770679,-0.947506517879914,
0.899998360166273));
#18424=CARTESIAN_POINT('Ctrl Pts',(0.352522341068277,-0.956064664041459,
0.899998150434084));
#18425=CARTESIAN_POINT('Ctrl Pts',(0.355135157141203,-0.964467130383873,
0.899998666502847));
#18426=CARTESIAN_POINT('Ctrl Pts',(0.358466575399326,-0.972608174091076,
0.89999965996049));
#18427=CARTESIAN_POINT('Ctrl Pts',(0.362538734686669,-0.982559379305286,
0.900000874313493));
#18428=CARTESIAN_POINT('Ctrl Pts',(0.367640276064737,-0.992015301694373,
0.90000291775694));
#18429=CARTESIAN_POINT('Ctrl Pts',(0.373711018494534,-1.00079214745216,
0.900002098461893));
#18430=CARTESIAN_POINT('Ctrl Pts',(0.3746124109217,-1.00209534593109,0.900001976811805));
#18431=CARTESIAN_POINT('Ctrl Pts',(0.375535256028145,-1.00338353399439,
0.900001785555943));
#18432=CARTESIAN_POINT('Ctrl Pts',(0.376479443106529,-1.00465606108108,
0.900001505529245));
#18433=CARTESIAN_POINT('Ctrl Pts',(0.380715143239362,-1.01036472123276,
0.900000249306668));
#18434=CARTESIAN_POINT('Ctrl Pts',(0.38537983051291,-1.01575881671377,0.899997265714102));
#18435=CARTESIAN_POINT('Ctrl Pts',(0.390428509023093,-1.02081078987204,
0.899994288896867));
#18436=CARTESIAN_POINT('Ctrl Pts',(0.398043974952909,-1.02843122547465,
0.899989798642598));
#18437=CARTESIAN_POINT('Ctrl Pts',(0.406453848296673,-1.0351976329321,0.899985566096));
#18438=CARTESIAN_POINT('Ctrl Pts',(0.415484607049401,-1.04103374418621,
0.899984276342262));
#18439=CARTESIAN_POINT('Ctrl Pts',(0.421222938370041,-1.04474213026064,
0.899983456806));
#18440=CARTESIAN_POINT('Ctrl Pts',(0.427212893823217,-1.04807424787086,
0.899983742291921));
#18441=CARTESIAN_POINT('Ctrl Pts',(0.433415948881005,-1.05100146303553,
0.899985033489932));
#18442=CARTESIAN_POINT('Ctrl Pts',(0.443112479013355,-1.05557724541753,
0.899987051872858));
#18443=CARTESIAN_POINT('Ctrl Pts',(0.453235937005982,-1.05912207412747,
0.899991654125809));
#18444=CARTESIAN_POINT('Ctrl Pts',(0.463629957379397,-1.06154692150368,
0.899995467994069));
#18445=CARTESIAN_POINT('Ctrl Pts',(0.470358492676306,-1.06311663856929,
0.899997936889288));
#18446=CARTESIAN_POINT('Ctrl Pts',(0.477201035001208,-1.06421620326297,
0.899999999975707));
#18447=CARTESIAN_POINT('Ctrl Pts',(0.484117964332956,-1.06481006947648,
0.9));
#18448=CARTESIAN_POINT('Ctrl Pts',(0.484117964332957,-1.06481006947648,
0.9));
#18449=CARTESIAN_POINT('Ctrl Pts',(0.486287923702977,-1.06263941570101,
0.941506444170342));
#18450=CARTESIAN_POINT('Ctrl Pts',(0.488457876548035,-1.06046876718106,
0.983012888930867));
#18451=CARTESIAN_POINT('Ctrl Pts',(0.490627822843887,-1.05829812393464,
1.02451933428366));
#18452=CARTESIAN_POINT('Ctrl Pts',(10.453005262311,-0.911780628641664,0.896713013448579));
#18453=CARTESIAN_POINT('Ctrl Pts',(10.4507783882972,-0.909557391891849,
0.939204300891032));
#18454=CARTESIAN_POINT('Ctrl Pts',(10.4485515142709,-0.907334159758067,
0.981695588574342));
#18455=CARTESIAN_POINT('Ctrl Pts',(10.4463246402318,-0.905110932257974,
1.02418687649944));
#18456=CARTESIAN_POINT('Ctrl Pts',(10.4528874757217,-0.954853661617317,
0.898960515458773));
#18457=CARTESIAN_POINT('Ctrl Pts',(10.4506605772126,-0.952629688741643,
0.941451759962203));
#18458=CARTESIAN_POINT('Ctrl Pts',(10.4484337586651,-0.950405759674027,
0.983943010977281));
#18459=CARTESIAN_POINT('Ctrl Pts',(10.4462068600709,-0.94818179413378,1.02643425584837));
#18460=CARTESIAN_POINT('Ctrl Pts',(10.4180804799687,-1.02952167699519,0.901043151378083));
#18461=CARTESIAN_POINT('Ctrl Pts',(10.4158548456208,-1.02729651565793,0.943534394542847));
#18462=CARTESIAN_POINT('Ctrl Pts',(10.413629193759,-1.02507134540722,0.986025636297673));
#18463=CARTESIAN_POINT('Ctrl Pts',(10.4114035625395,-1.02284618829514,1.02851687981561));
#18464=CARTESIAN_POINT('Ctrl Pts',(10.3442106925096,-1.05932070834318,0.898730950115076));
#18465=CARTESIAN_POINT('Ctrl Pts',(10.3419870251366,-1.05709644901815,0.941222341385074));
#18466=CARTESIAN_POINT('Ctrl Pts',(10.3397633429135,-1.0548722146549,0.983713733185165));
#18467=CARTESIAN_POINT('Ctrl Pts',(10.3375396837912,-1.05264796171536,1.0262051251811));
#18468=CARTESIAN_POINT('Ctrl Pts',(10.3119612275562,-1.06129600030118,0.897144178853313));
#18469=CARTESIAN_POINT('Ctrl Pts',(10.309738142952,-1.05907253204827,0.939635641919598));
#18470=CARTESIAN_POINT('Ctrl Pts',(10.3075150632522,-1.05684906796687,0.982127105440503));
#18471=CARTESIAN_POINT('Ctrl Pts',(10.3052919884757,-1.05462560807237,1.02461856941773));
#18472=CARTESIAN_POINT('',(10.3118118156214,-1.06114656258054,0.9));
#18473=CARTESIAN_POINT('Ctrl Pts',(10.3053025283406,-1.05463614976313,1.02441711227736));
#18474=CARTESIAN_POINT('Ctrl Pts',(10.3074722860834,-1.05680628338526,0.982944741084074));
#18475=CARTESIAN_POINT('Ctrl Pts',(10.3096420485163,-1.05897642099582,0.941472370325482));
#18476=CARTESIAN_POINT('Ctrl Pts',(10.3118118156214,-1.06114656258054,0.900000000000001));
#18477=CARTESIAN_POINT('Ctrl Pts',(10.3118118156214,-1.06114656258054,0.900000000000001));
#18478=CARTESIAN_POINT('Ctrl Pts',(10.322549369014,-1.06051812817027,0.899999999998837));
#18479=CARTESIAN_POINT('Ctrl Pts',(10.3331651969327,-1.05870347076406,0.899998279675625));
#18480=CARTESIAN_POINT('Ctrl Pts',(10.3434824690201,-1.05579899810317,0.899997678781422));
#18481=CARTESIAN_POINT('Ctrl Pts',(10.3519099591122,-1.05342652848477,0.899997187951103));
#18482=CARTESIAN_POINT('Ctrl Pts',(10.3601388923794,-1.05032564389788,0.899997411230107));
#18483=CARTESIAN_POINT('Ctrl Pts',(10.368065652211,-1.04652424300033,0.899998227267474));
#18484=CARTESIAN_POINT('Ctrl Pts',(10.3777613500057,-1.04187452040475,0.89999922541197));
#18485=CARTESIAN_POINT('Ctrl Pts',(10.3869029298231,-1.0362271920453,0.900001226887481));
#18486=CARTESIAN_POINT('Ctrl Pts',(10.3953114913929,-1.02965576012812,0.900000692598515));
#18487=CARTESIAN_POINT('Ctrl Pts',(10.3970212347867,-1.0283195669856,0.900000583959597));
#18488=CARTESIAN_POINT('Ctrl Pts',(10.3987005924826,-1.02694501523934,0.900000358370781));
#18489=CARTESIAN_POINT('Ctrl Pts',(10.4003479139729,-1.02553250004787,0.899999966744969));
#18490=CARTESIAN_POINT('Ctrl Pts',(10.4052955867552,-1.02129005981461,0.899998790510468));
#18491=CARTESIAN_POINT('Ctrl Pts',(10.4099546972526,-1.01670546321193,0.899996154952331));
#18492=CARTESIAN_POINT('Ctrl Pts',(10.4143066574475,-1.01181472964029,0.899993423989004));
#18493=CARTESIAN_POINT('Ctrl Pts',(10.4214686344271,-1.00376609875091,0.899988929670213));
#18494=CARTESIAN_POINT('Ctrl Pts',(10.4277268376922,-0.994973664259554,
0.899984438878373));
#18495=CARTESIAN_POINT('Ctrl Pts',(10.4330201329469,-0.985617486073369,
0.899982870029797));
#18496=CARTESIAN_POINT('Ctrl Pts',(10.4367196060238,-0.979078472540647,
0.89998177356478));
#18497=CARTESIAN_POINT('Ctrl Pts',(10.4399470827666,-0.972263038755175,
0.89998201356482));
#18498=CARTESIAN_POINT('Ctrl Pts',(10.4426687152005,-0.965225084739993,
0.899983510148066));
#18499=CARTESIAN_POINT('Ctrl Pts',(10.4465375225522,-0.955220615401818,
0.899985637544916));
#18500=CARTESIAN_POINT('Ctrl Pts',(10.4493477346146,-0.944866529467853,
0.899990392295554));
#18501=CARTESIAN_POINT('Ctrl Pts',(10.4510237312406,-0.934325606572895,
0.899994522211612));
#18502=CARTESIAN_POINT('Ctrl Pts',(10.452215546318,-0.926829869027476,0.899997459029114));
#18503=CARTESIAN_POINT('Ctrl Pts',(10.452832998309,-0.919238945488459,0.899999999973399));
#18504=CARTESIAN_POINT('Ctrl Pts',(10.4528329986453,-0.911608646352004,
0.9));
#18505=CARTESIAN_POINT('Origin',(5.4,0.,0.9));
#18506=CARTESIAN_POINT('Ctrl Pts',(10.3118118156214,-1.06114656258054,0.9));
#18507=CARTESIAN_POINT('Ctrl Pts',(7.03591386519191,-1.25287427294368,0.9));
#18508=CARTESIAN_POINT('Ctrl Pts',(3.76001591476243,-1.34606837492147,0.9));
#18509=CARTESIAN_POINT('Ctrl Pts',(0.484117964332957,-1.06481006947648,
0.9));
#18510=CARTESIAN_POINT('Ctrl Pts',(10.3118118156214,-1.06114656258054,0.9));
#18511=CARTESIAN_POINT('Ctrl Pts',(10.3096972650911,-1.05897130198467,0.94150644476122));
#18512=CARTESIAN_POINT('Ctrl Pts',(10.3075827145608,-1.0567960413888,0.98301288952244));
#18513=CARTESIAN_POINT('Ctrl Pts',(10.3054681640305,-1.05462078079293,1.02451933428366));
#18514=CARTESIAN_POINT('Ctrl Pts',(7.03591386519191,-1.25287427294368,0.9));
#18515=CARTESIAN_POINT('Ctrl Pts',(7.03520959909601,-1.25069901234781,0.94150644476122));
#18516=CARTESIAN_POINT('Ctrl Pts',(7.03450533300011,-1.24852375175194,0.98301288952244));
#18517=CARTESIAN_POINT('Ctrl Pts',(7.03380106690421,-1.24634849115607,1.02451933428366));
#18518=CARTESIAN_POINT('Ctrl Pts',(3.76001591476244,-1.34606837492147,0.9));
#18519=CARTESIAN_POINT('Ctrl Pts',(3.76072193310095,-1.3438931143256,0.94150644476122));
#18520=CARTESIAN_POINT('Ctrl Pts',(3.76142795143946,-1.34171785372973,0.98301288952244));
#18521=CARTESIAN_POINT('Ctrl Pts',(3.76213396977796,-1.33954259313386,1.02451933428366));
#18522=CARTESIAN_POINT('Ctrl Pts',(0.484117964332957,-1.06481006947648,
0.9));
#18523=CARTESIAN_POINT('Ctrl Pts',(0.486234267105876,-1.06263480888061,
0.94150644476122));
#18524=CARTESIAN_POINT('Ctrl Pts',(0.488350569878795,-1.06045954828474,
0.98301288952244));
#18525=CARTESIAN_POINT('Ctrl Pts',(0.490466872651714,-1.05828428768887,
1.02451933428366));
#18526=CARTESIAN_POINT('',(0.,0.,0.));
#18527=CARTESIAN_POINT('',(0.,0.,0.));
#18528=CARTESIAN_POINT('',(2.,0.,0.6));
#18529=CARTESIAN_POINT('',(2.,0.,-0.84));
#18530=CARTESIAN_POINT('',(0.,0.,0.));
#18531=CARTESIAN_POINT('',(8.8,0.,0.6));
#18532=CARTESIAN_POINT('',(8.8,0.,-0.84));
#18533=CARTESIAN_POINT('',(0.,0.,0.));
#18534=CARTESIAN_POINT('',(0.,0.,0.));
#18535=CARTESIAN_POINT('Origin',(0.,0.,0.));
#18536=CARTESIAN_POINT('',(-0.41,-5.02105187650415E-17,0.1));
#18537=CARTESIAN_POINT('Origin',(0.,0.,0.1));
#18538=CARTESIAN_POINT('',(-0.41,-5.02105187650415E-17,0.));
#18539=CARTESIAN_POINT('',(-0.41,-5.02105187650415E-17,0.));
#18540=CARTESIAN_POINT('Origin',(0.,0.,0.));
#18541=CARTESIAN_POINT('Origin',(0.,0.,0.));
#18542=CARTESIAN_POINT('',(-0.6,-7.34788079488412E-17,0.1));
#18543=CARTESIAN_POINT('Origin',(0.,0.,0.1));
#18544=CARTESIAN_POINT('',(-0.6,-7.34788079488412E-17,0.));
#18545=CARTESIAN_POINT('',(-0.6,-7.34788079488412E-17,0.));
#18546=CARTESIAN_POINT('Origin',(0.,0.,0.));
#18547=CARTESIAN_POINT('Origin',(0.,0.,0.1));
#18548=CARTESIAN_POINT('Origin',(0.,0.,0.));
#18549=CARTESIAN_POINT('',(0.,0.,0.));
#18550=CARTESIAN_POINT('',(4.,-2.5,0.3));
#18551=CARTESIAN_POINT('',(0.,0.,0.));
#18552=CARTESIAN_POINT('',(0.,0.,0.));
#18553=CARTESIAN_POINT('',(0.,0.,0.6));
#18554=CARTESIAN_POINT('',(0.,0.,0.7));
#18555=CARTESIAN_POINT('',(4.,2.5,-0.3));
#18556=CARTESIAN_POINT('',(0.,0.,-0.7));
#18557=UNCERTAINTY_MEASURE_WITH_UNIT(LENGTH_MEASURE(0.001),#18581,
'DISTANCE_ACCURACY_VALUE',
'Maximum model space distance between geometric entities at asserted c
onnectivities');
#18558=UNCERTAINTY_MEASURE_WITH_UNIT(LENGTH_MEASURE(0.001),#18581,
'DISTANCE_ACCURACY_VALUE',
'Maximum model space distance between geometric entities at asserted c
onnectivities');
#18559=UNCERTAINTY_MEASURE_WITH_UNIT(LENGTH_MEASURE(0.001),#18581,
'DISTANCE_ACCURACY_VALUE',
'Maximum model space distance between geometric entities at asserted c
onnectivities');
#18560=UNCERTAINTY_MEASURE_WITH_UNIT(LENGTH_MEASURE(0.001),#18581,
'DISTANCE_ACCURACY_VALUE',
'Maximum model space distance between geometric entities at asserted c
onnectivities');
#18561=UNCERTAINTY_MEASURE_WITH_UNIT(LENGTH_MEASURE(0.001),#18581,
'DISTANCE_ACCURACY_VALUE',
'Maximum model space distance between geometric entities at asserted c
onnectivities');
#18562=UNCERTAINTY_MEASURE_WITH_UNIT(LENGTH_MEASURE(0.001),#18581,
'DISTANCE_ACCURACY_VALUE',
'Maximum model space distance between geometric entities at asserted c
onnectivities');
#18563=UNCERTAINTY_MEASURE_WITH_UNIT(LENGTH_MEASURE(0.001),#18581,
'DISTANCE_ACCURACY_VALUE',
'Maximum model space distance between geometric entities at asserted c
onnectivities');
#18564=UNCERTAINTY_MEASURE_WITH_UNIT(LENGTH_MEASURE(0.001),#18581,
'DISTANCE_ACCURACY_VALUE',
'Maximum model space distance between geometric entities at asserted c
onnectivities');
#18565=UNCERTAINTY_MEASURE_WITH_UNIT(LENGTH_MEASURE(0.001),#18581,
'DISTANCE_ACCURACY_VALUE',
'Maximum model space distance between geometric entities at asserted c
onnectivities');
#18566=UNCERTAINTY_MEASURE_WITH_UNIT(LENGTH_MEASURE(0.001),#18581,
'DISTANCE_ACCURACY_VALUE',
'Maximum model space distance between geometric entities at asserted c
onnectivities');
#18567=UNCERTAINTY_MEASURE_WITH_UNIT(LENGTH_MEASURE(0.001),#18581,
'DISTANCE_ACCURACY_VALUE',
'Maximum model space distance between geometric entities at asserted c
onnectivities');
#18568=UNCERTAINTY_MEASURE_WITH_UNIT(LENGTH_MEASURE(0.001),#18581,
'DISTANCE_ACCURACY_VALUE',
'Maximum model space distance between geometric entities at asserted c
onnectivities');
#18569=(
GEOMETRIC_REPRESENTATION_CONTEXT(3)
GLOBAL_UNCERTAINTY_ASSIGNED_CONTEXT((#18557))
GLOBAL_UNIT_ASSIGNED_CONTEXT((#18581,#18583,#18584))
REPRESENTATION_CONTEXT('','3D')
);
#18570=(
GEOMETRIC_REPRESENTATION_CONTEXT(3)
GLOBAL_UNCERTAINTY_ASSIGNED_CONTEXT((#18558))
GLOBAL_UNIT_ASSIGNED_CONTEXT((#18581,#18583,#18584))
REPRESENTATION_CONTEXT('','3D')
);
#18571=(
GEOMETRIC_REPRESENTATION_CONTEXT(3)
GLOBAL_UNCERTAINTY_ASSIGNED_CONTEXT((#18559))
GLOBAL_UNIT_ASSIGNED_CONTEXT((#18581,#18583,#18584))
REPRESENTATION_CONTEXT('','3D')
);
#18572=(
GEOMETRIC_REPRESENTATION_CONTEXT(3)
GLOBAL_UNCERTAINTY_ASSIGNED_CONTEXT((#18560))
GLOBAL_UNIT_ASSIGNED_CONTEXT((#18581,#18583,#18584))
REPRESENTATION_CONTEXT('','3D')
);
#18573=(
GEOMETRIC_REPRESENTATION_CONTEXT(3)
GLOBAL_UNCERTAINTY_ASSIGNED_CONTEXT((#18561))
GLOBAL_UNIT_ASSIGNED_CONTEXT((#18581,#18583,#18584))
REPRESENTATION_CONTEXT('','3D')
);
#18574=(
GEOMETRIC_REPRESENTATION_CONTEXT(3)
GLOBAL_UNCERTAINTY_ASSIGNED_CONTEXT((#18562))
GLOBAL_UNIT_ASSIGNED_CONTEXT((#18581,#18583,#18584))
REPRESENTATION_CONTEXT('','3D')
);
#18575=(
GEOMETRIC_REPRESENTATION_CONTEXT(3)
GLOBAL_UNCERTAINTY_ASSIGNED_CONTEXT((#18563))
GLOBAL_UNIT_ASSIGNED_CONTEXT((#18581,#18583,#18584))
REPRESENTATION_CONTEXT('','3D')
);
#18576=(
GEOMETRIC_REPRESENTATION_CONTEXT(3)
GLOBAL_UNCERTAINTY_ASSIGNED_CONTEXT((#18564))
GLOBAL_UNIT_ASSIGNED_CONTEXT((#18581,#18583,#18584))
REPRESENTATION_CONTEXT('','3D')
);
#18577=(
GEOMETRIC_REPRESENTATION_CONTEXT(3)
GLOBAL_UNCERTAINTY_ASSIGNED_CONTEXT((#18565))
GLOBAL_UNIT_ASSIGNED_CONTEXT((#18581,#18583,#18584))
REPRESENTATION_CONTEXT('','3D')
);
#18578=(
GEOMETRIC_REPRESENTATION_CONTEXT(3)
GLOBAL_UNCERTAINTY_ASSIGNED_CONTEXT((#18566))
GLOBAL_UNIT_ASSIGNED_CONTEXT((#18581,#18583,#18584))
REPRESENTATION_CONTEXT('','3D')
);
#18579=(
GEOMETRIC_REPRESENTATION_CONTEXT(3)
GLOBAL_UNCERTAINTY_ASSIGNED_CONTEXT((#18567))
GLOBAL_UNIT_ASSIGNED_CONTEXT((#18581,#18583,#18584))
REPRESENTATION_CONTEXT('','3D')
);
#18580=(
GEOMETRIC_REPRESENTATION_CONTEXT(3)
GLOBAL_UNCERTAINTY_ASSIGNED_CONTEXT((#18568))
GLOBAL_UNIT_ASSIGNED_CONTEXT((#18581,#18583,#18584))
REPRESENTATION_CONTEXT('','3D')
);
#18581=(
LENGTH_UNIT()
NAMED_UNIT(*)
SI_UNIT(.CENTI.,.METRE.)
);
#18582=(
LENGTH_UNIT()
NAMED_UNIT(*)
SI_UNIT($,.METRE.)
);
#18583=(
NAMED_UNIT(*)
PLANE_ANGLE_UNIT()
SI_UNIT($,.RADIAN.)
);
#18584=(
NAMED_UNIT(*)
SI_UNIT($,.STERADIAN.)
SOLID_ANGLE_UNIT()
);
#18585=SHAPE_DEFINITION_REPRESENTATION(#18596,#18623);
#18586=SHAPE_DEFINITION_REPRESENTATION(#18597,#18624);
#18587=SHAPE_DEFINITION_REPRESENTATION(#18598,#18625);
#18588=SHAPE_DEFINITION_REPRESENTATION(#18599,#18626);
#18589=SHAPE_DEFINITION_REPRESENTATION(#18600,#18627);
#18590=SHAPE_DEFINITION_REPRESENTATION(#18601,#18628);
#18591=SHAPE_DEFINITION_REPRESENTATION(#18602,#18629);
#18592=SHAPE_DEFINITION_REPRESENTATION(#18603,#18630);
#18593=SHAPE_DEFINITION_REPRESENTATION(#18604,#18631);
#18594=SHAPE_DEFINITION_REPRESENTATION(#18605,#18632);
#18595=SHAPE_DEFINITION_REPRESENTATION(#18614,#18633);
#18596=PRODUCT_DEFINITION_SHAPE('',$,#18635);
#18597=PRODUCT_DEFINITION_SHAPE('',$,#18636);
#18598=PRODUCT_DEFINITION_SHAPE('',$,#18637);
#18599=PRODUCT_DEFINITION_SHAPE('',$,#18638);
#18600=PRODUCT_DEFINITION_SHAPE('',$,#18639);
#18601=PRODUCT_DEFINITION_SHAPE('',$,#18640);
#18602=PRODUCT_DEFINITION_SHAPE('',$,#18641);
#18603=PRODUCT_DEFINITION_SHAPE('',$,#18642);
#18604=PRODUCT_DEFINITION_SHAPE('',$,#18643);
#18605=PRODUCT_DEFINITION_SHAPE('',$,#18644);
#18606=PRODUCT_DEFINITION_SHAPE($,$,#59);
#18607=PRODUCT_DEFINITION_SHAPE($,$,#60);
#18608=PRODUCT_DEFINITION_SHAPE($,$,#61);
#18609=PRODUCT_DEFINITION_SHAPE($,$,#62);
#18610=PRODUCT_DEFINITION_SHAPE($,$,#63);
#18611=PRODUCT_DEFINITION_SHAPE($,$,#64);
#18612=PRODUCT_DEFINITION_SHAPE($,$,#65);
#18613=PRODUCT_DEFINITION_SHAPE($,$,#66);
#18614=PRODUCT_DEFINITION_SHAPE('',$,#18645);
#18615=PRODUCT_DEFINITION_SHAPE($,$,#67);
#18616=PRODUCT_DEFINITION_SHAPE($,$,#68);
#18617=PRODUCT_DEFINITION_SHAPE($,$,#69);
#18618=PRODUCT_DEFINITION_SHAPE($,$,#70);
#18619=PRODUCT_DEFINITION_SHAPE($,$,#71);
#18620=PRODUCT_DEFINITION_SHAPE($,$,#72);
#18621=PRODUCT_DEFINITION_SHAPE($,$,#73);
#18622=PRODUCT_DEFINITION_SHAPE($,$,#74);
#18623=SHAPE_REPRESENTATION('',(#6653,#7126,#7127,#7128,#7129,#7130,#7131,
#7132,#7133),#18569);
#18624=SHAPE_REPRESENTATION('',(#6654),#18570);
#18625=SHAPE_REPRESENTATION('',(#6692),#18571);
#18626=SHAPE_REPRESENTATION('',(#6710),#18572);
#18627=SHAPE_REPRESENTATION('',(#6721,#7109,#7110,#7111,#7112,#7113,#7114,
#7115,#7116),#18573);
#18628=SHAPE_REPRESENTATION('',(#6722),#18574);
#18629=SHAPE_REPRESENTATION('',(#6832),#18575);
#18630=SHAPE_REPRESENTATION('',(#6948),#18576);
#18631=SHAPE_REPRESENTATION('',(#7030),#18577);
#18632=SHAPE_REPRESENTATION('',(#7056),#18578);
#18633=SHAPE_REPRESENTATION('',(#7117),#18579);
#18634=PRODUCT_DEFINITION_CONTEXT('part definition',#18669,'design');
#18635=PRODUCT_DEFINITION('TOOL-023','TOOL-023',#18646,#18634);
#18636=PRODUCT_DEFINITION('Forged jaw and handle',
'Forged jaw and handle',#18647,#18634);
#18637=PRODUCT_DEFINITION('Shoulder pivot pin','Shoulder pivot pin',#18648,
#18634);
#18638=PRODUCT_DEFINITION('Pivot retaining ring','Pivot retaining ring',
#18649,#18634);
#18639=PRODUCT_DEFINITION('GRP-001','Grip module',#18650,#18634);
#18640=PRODUCT_DEFINITION('2026-11-10-05-09-36-725',
'Upper structural shell',#18651,#18634);
#18641=PRODUCT_DEFINITION('2026-11-10-05-09-36-729',
'Lower structural shell',#18652,#18634);
#18642=PRODUCT_DEFINITION('2026-11-10-05-09-36-733',
'Socket head cap screw M3x16',#18653,#18634);
#18643=PRODUCT_DEFINITION('2026-11-10-05-09-36-734','Hex nut M3',#18654,
#18634);
#18644=PRODUCT_DEFINITION('2026-11-10-05-09-36-736','Soft grip layer',#18655,
#18634);
#18645=PRODUCT_DEFINITION('Pivot thrust washer','Pivot thrust washer',#18656,
#18634);
#18646=PRODUCT_DEFINITION_FORMATION('',$,#18671);
#18647=PRODUCT_DEFINITION_FORMATION('',$,#18672);
#18648=PRODUCT_DEFINITION_FORMATION('',$,#18673);
#18649=PRODUCT_DEFINITION_FORMATION('',$,#18674);
#18650=PRODUCT_DEFINITION_FORMATION('',$,#18675);
#18651=PRODUCT_DEFINITION_FORMATION('',$,#18676);
#18652=PRODUCT_DEFINITION_FORMATION('',$,#18677);
#18653=PRODUCT_DEFINITION_FORMATION('',$,#18678);
#18654=PRODUCT_DEFINITION_FORMATION('',$,#18679);
#18655=PRODUCT_DEFINITION_FORMATION('',$,#18680);
#18656=PRODUCT_DEFINITION_FORMATION('',$,#18681);
#18657=PRODUCT_RELATED_PRODUCT_CATEGORY('TOOL-023','TOOL-023',(#18671));
#18658=PRODUCT_RELATED_PRODUCT_CATEGORY('Forged jaw and handle',
'Forged jaw and handle',(#18672));
#18659=PRODUCT_RELATED_PRODUCT_CATEGORY('Shoulder pivot pin',
'Shoulder pivot pin',(#18673));
#18660=PRODUCT_RELATED_PRODUCT_CATEGORY('Pivot retaining ring',
'Pivot retaining ring',(#18674));
#18661=PRODUCT_RELATED_PRODUCT_CATEGORY('Grip module','Grip module',(#18675));
#18662=PRODUCT_RELATED_PRODUCT_CATEGORY('Upper structural shell',
'Upper structural shell',(#18676));
#18663=PRODUCT_RELATED_PRODUCT_CATEGORY('Lower structural shell',
'Lower structural shell',(#18677));
#18664=PRODUCT_RELATED_PRODUCT_CATEGORY('Socket head cap screw M3x16',
'Socket head cap screw M3x16',(#18678));
#18665=PRODUCT_RELATED_PRODUCT_CATEGORY('Hex nut M3','Hex nut M3',(#18679));
#18666=PRODUCT_RELATED_PRODUCT_CATEGORY('Soft grip layer',
'Soft grip layer',(#18680));
#18667=PRODUCT_RELATED_PRODUCT_CATEGORY('Pivot thrust washer',
'Pivot thrust washer',(#18681));
#18668=APPLICATION_PROTOCOL_DEFINITION('international standard',
'automotive_design',2009,#18669);
#18669=APPLICATION_CONTEXT(
'Core Data for Automotive Mechanical Design Process');
#18670=PRODUCT_CONTEXT('part definition',#18669,'mechanical');
#18671=PRODUCT('TOOL-023','TOOL-023',$,(#18670));
#18672=PRODUCT('Forged jaw and handle','Forged jaw and handle',$,(#18670));
#18673=PRODUCT('Shoulder pivot pin','Shoulder pivot pin',$,(#18670));
#18674=PRODUCT('Pivot retaining ring','Pivot retaining ring',$,(#18670));
#18675=PRODUCT('GRP-001','Grip module',$,(#18670));
#18676=PRODUCT('2026-11-10-05-09-36-725','Upper structural shell',$,(#18670));
#18677=PRODUCT('2026-11-10-05-09-36-729','Lower structural shell',$,(#18670));
#18678=PRODUCT('2026-11-10-05-09-36-733','Socket head cap screw M3x16',
$,(#18670));
#18679=PRODUCT('2026-11-10-05-09-36-734','Hex nut M3',$,(#18670));
#18680=PRODUCT('2026-11-10-05-09-36-736','Soft grip layer',$,(#18670));
#18681=PRODUCT('Pivot thrust washer','Pivot thrust washer',$,(#18670));
#18682=PRESENTATION_STYLE_ASSIGNMENT((#18690));
#18683=PRESENTATION_STYLE_ASSIGNMENT((#18691));
#18684=PRESENTATION_STYLE_ASSIGNMENT((#18692));
#18685=PRESENTATION_STYLE_ASSIGNMENT((#18693));
#18686=PRESENTATION_STYLE_ASSIGNMENT((#18694));
#18687=PRESENTATION_STYLE_ASSIGNMENT((#18695));
#18688=PRESENTATION_STYLE_ASSIGNMENT((#18696));
#18689=PRESENTATION_STYLE_ASSIGNMENT((#18697));
#18690=SURFACE_STYLE_USAGE(.BOTH.,#18698);
#18691=SURFACE_STYLE_USAGE(.BOTH.,#18699);
#18692=SURFACE_STYLE_USAGE(.BOTH.,#18700);
#18693=SURFACE_STYLE_USAGE(.BOTH.,#18701);
#18694=SURFACE_STYLE_USAGE(.BOTH.,#18702);
#18695=SURFACE_STYLE_USAGE(.BOTH.,#18703);
#18696=SURFACE_STYLE_USAGE(.BOTH.,#18704);
#18697=SURFACE_STYLE_USAGE(.BOTH.,#18705);
#18698=SURFACE_SIDE_STYLE('',(#18706));
#18699=SURFACE_SIDE_STYLE('',(#18707));
#18700=SURFACE_SIDE_STYLE('',(#18708));
#18701=SURFACE_SIDE_STYLE('',(#18709));
#18702=SURFACE_SIDE_STYLE('',(#18710));
#18703=SURFACE_SIDE_STYLE('',(#18711));
#18704=SURFACE_SIDE_STYLE('',(#18712));
#18705=SURFACE_SIDE_STYLE('',(#18713));
#18706=SURFACE_STYLE_FILL_AREA(#18714);
#18707=SURFACE_STYLE_FILL_AREA(#18715);
#18708=SURFACE_STYLE_FILL_AREA(#18716);
#18709=SURFACE_STYLE_FILL_AREA(#18717);
#18710=SURFACE_STYLE_FILL_AREA(#18718);
#18711=SURFACE_STYLE_FILL_AREA(#18719);
#18712=SURFACE_STYLE_FILL_AREA(#18720);
#18713=SURFACE_STYLE_FILL_AREA(#18721);
#18714=FILL_AREA_STYLE('Steel - Satin',(#18722));
#18715=FILL_AREA_STYLE('Tool steel gray',(#18723));
#18716=FILL_AREA_STYLE('Pivot dark gray',(#18724));
#18717=FILL_AREA_STYLE('Dark gray',(#18725));
#18718=FILL_AREA_STYLE('Structural dark blue',(#18726));
#18719=FILL_AREA_STYLE('Fastener gray',(#18727));
#18720=FILL_AREA_STYLE('Sky blue soft grip',(#18728));
#18721=FILL_AREA_STYLE('Washer gray',(#18729));
#18722=FILL_AREA_STYLE_COLOUR('Steel - Satin',#18730);
#18723=FILL_AREA_STYLE_COLOUR('Tool steel gray',#18731);
#18724=FILL_AREA_STYLE_COLOUR('Pivot dark gray',#18732);
#18725=FILL_AREA_STYLE_COLOUR('Dark gray',#18733);
#18726=FILL_AREA_STYLE_COLOUR('Structural dark blue',#18734);
#18727=FILL_AREA_STYLE_COLOUR('Fastener gray',#18735);
#18728=FILL_AREA_STYLE_COLOUR('Sky blue soft grip',#18736);
#18729=FILL_AREA_STYLE_COLOUR('Washer gray',#18737);
#18730=COLOUR_RGB('Steel - Satin',0.627450980392157,0.627450980392157,0.627450980392157);
#18731=COLOUR_RGB('Tool steel gray',0.607843137254902,0.643137254901961,
0.698039215686274);
#18732=COLOUR_RGB('Pivot dark gray',0.27843137254902,0.309803921568627,
0.352941176470588);
#18733=COLOUR_RGB('Dark gray',0.250980392156863,0.282352941176471,0.32156862745098);
#18734=COLOUR_RGB('Structural dark blue',0.0901960784313725,0.270588235294118,
0.513725490196078);
#18735=COLOUR_RGB('Fastener gray',0.607843137254902,0.643137254901961,0.698039215686274);
#18736=COLOUR_RGB('Sky blue soft grip',0.317647058823529,0.686274509803922,
0.890196078431372);
#18737=COLOUR_RGB('Washer gray',0.725490196078431,0.752941176470588,0.792156862745098);
ENDSEC;
END-ISO-10303-21;
